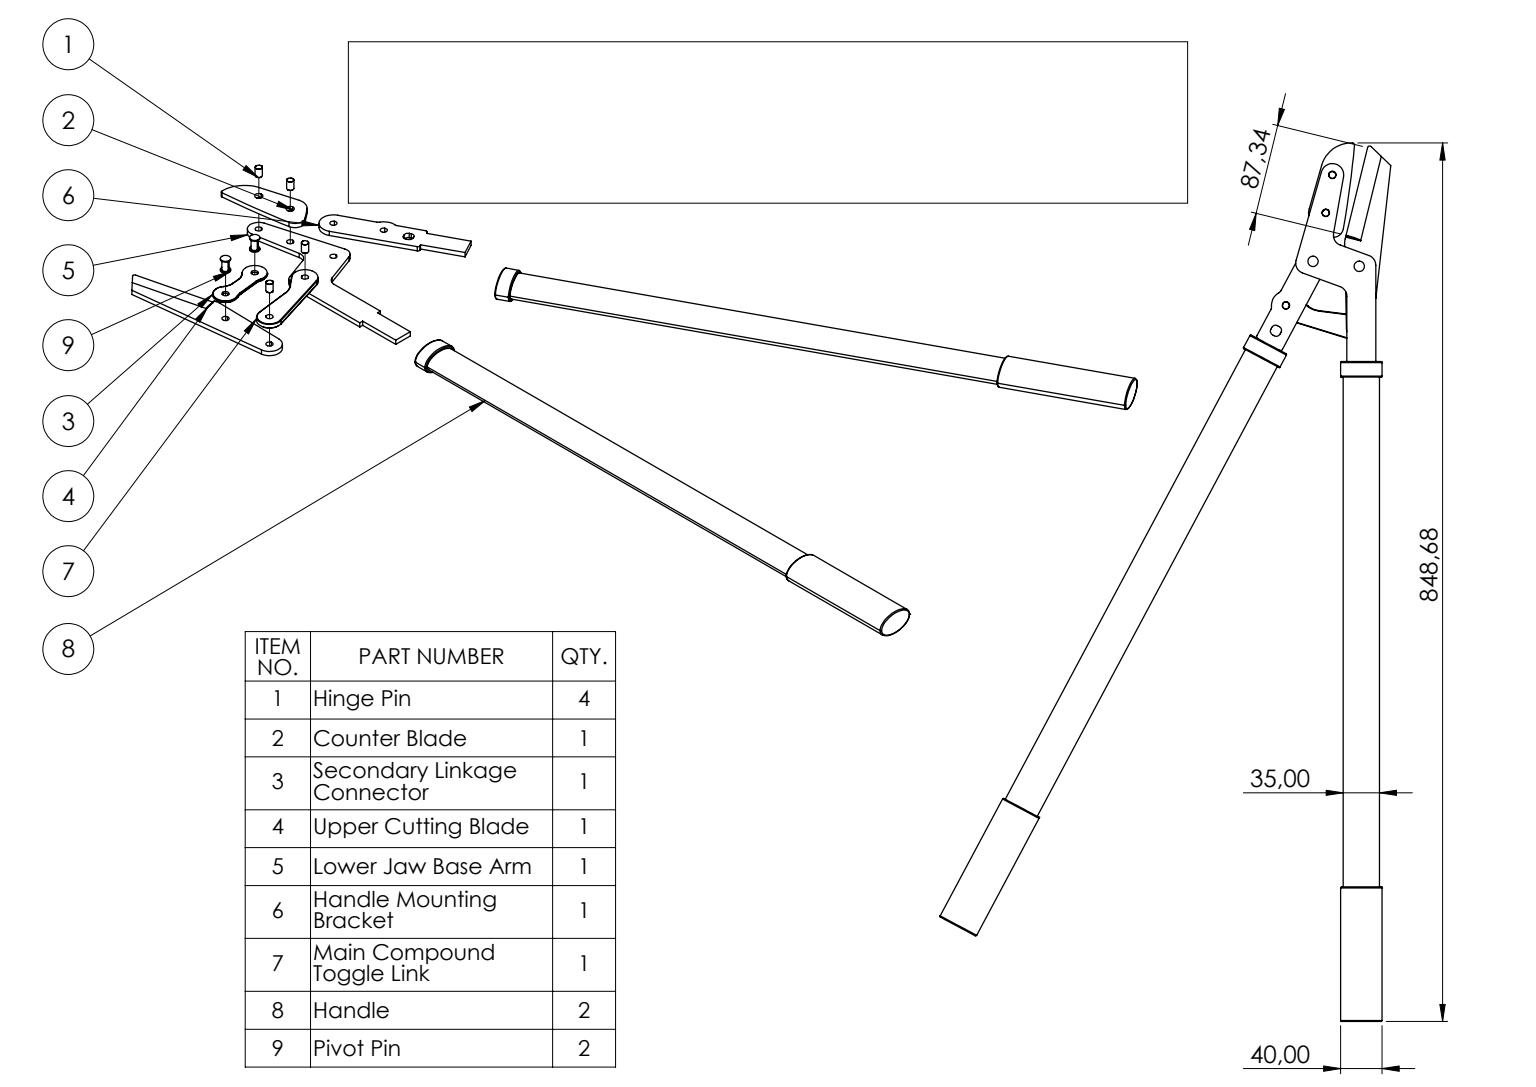
ISO-10303-21;
HEADER;
FILE_DESCRIPTION (('STEP AP214'),
    '1' );
FILE_NAME ('MAS-686',
    '2026-10-06T08:24:18',
    ( '' ),
    ( '' ),
    'SwSTEP 2.0',
    'SolidWorks 2020',
    '' );
FILE_SCHEMA (( 'AUTOMOTIVE_DESIGN' ));
ENDSEC;

DATA;
#1 = B_SPLINE_CURVE_WITH_KNOTS ( 'NONE', 3,
 ( #1947, #5214, #5583, #6285 ),
 .UNSPECIFIED., .F., .F.,
 ( 4, 4 ),
 ( 0.000000000000000000, 1.000000000000000000 ),
 .UNSPECIFIED. ) ;
#2 = DIRECTION ( 'NONE',  ( -0.000000000000000000, 1.000000000000000000, 0.000000000000000000 ) ) ;
#3 = AXIS2_PLACEMENT_3D ( 'NONE', #1835, #8382, #7525 ) ;
#4 = CARTESIAN_POINT ( 'NONE',  ( 15.24035984457677628, 4.192874667847209302, 315.0000000000000000 ) ) ;
#5 = CARTESIAN_POINT ( 'NONE',  ( 9.254661647337838914, -11.09380704494734360, -303.4999999999996589 ) ) ;
#6 = CARTESIAN_POINT ( 'NONE',  ( 16.58659719219999928, 2.947707964209000053, -314.6383426456000052 ) ) ;
#7 = SURFACE_SIDE_STYLE ('',( #8873 ) ) ;
#8 = CARTESIAN_POINT ( 'NONE',  ( -14.98500449093754483, -6.750000000000000000, -438.4247239981262396 ) ) ;
#9 = CARTESIAN_POINT ( 'NONE',  ( -1.582652182125599660, -2.660653890702000091, -435.1382991101020821 ) ) ;
#10 = ORIENTED_EDGE ( 'NONE', *, *, #9690, .T. ) ;
#11 = CARTESIAN_POINT ( 'NONE',  ( 14.97796429264999141, 8.396158284077998246, -317.0792622552969533 ) ) ;
#12 = AXIS2_PLACEMENT_3D ( 'NONE', #3802, #4074, #7998 ) ;
#13 = LINE ( 'NONE', #6569, #9092 ) ;
#14 = APPLICATION_CONTEXT ( 'automotive_design' ) ;
#15 = CARTESIAN_POINT ( 'NONE',  ( 4.345375235838000449, -11.20786428128000090, 320.0000000000000000 ) ) ;
#16 = CARTESIAN_POINT ( 'NONE',  ( -1.663986357696749074, -7.359447597713999478, -434.8428272099179708 ) ) ;
#17 = UNCERTAINTY_MEASURE_WITH_UNIT (LENGTH_MEASURE( 1.000000000000000082E-05 ), #9490, 'distance_accuracy_value', 'NONE');
#18 = CARTESIAN_POINT ( 'NONE',  ( -18.02719435607597021, -9.000000000000001776, -431.8467903975401896 ) ) ;
#19 = CARTESIAN_POINT ( 'NONE',  ( 12.11078853722071180, -6.646648371397081867, -315.0000000000000000 ) ) ;
#20 = ORIENTED_EDGE ( 'NONE', *, *, #8443, .F. ) ;
#21 = PLANE ( 'NONE',  #9517 ) ;
#22 = VERTEX_POINT ( 'NONE', #5856 ) ;
#23 = CARTESIAN_POINT ( 'NONE',  ( -16.90341843474000072, 5.241942252742000541, -317.4999999999989768 ) ) ;
#24 = VERTEX_POINT ( 'NONE', #8281 ) ;
#25 = AXIS2_PLACEMENT_3D ( 'NONE', #9737, #2431, #8928 ) ;
#26 = CARTESIAN_POINT ( 'NONE',  ( -6.686361683900003072, -11.78513185998999546, -303.6197174156509391 ) ) ;
#27 = EDGE_CURVE ( 'NONE', #6443, #1984, #9042, .T. ) ;
#28 = CARTESIAN_POINT ( 'NONE',  ( 9.022589772749004311, -9.990182113135000819, -317.4928077629770087 ) ) ;
#29 = CARTESIAN_POINT ( 'NONE',  ( 10.00000000000000000, 2.500000000000000000, -317.5000000000000000 ) ) ;
#30 = EDGE_CURVE ( 'NONE', #1105, #135, #3775, .T. ) ;
#31 = CARTESIAN_POINT ( 'NONE',  ( -18.56223039349998771, 4.700611568415998143, -303.6197174156520759 ) ) ;
#32 = CARTESIAN_POINT ( 'NONE',  ( -17.50000003227012613, 5.857864393370423528, 314.9999999999999432 ) ) ;
#33 = SHAPE_REPRESENTATION ( 'Main Compound Toggle Link', ( #2817 ), #8667 ) ;
#34 = EDGE_LOOP ( 'NONE', ( #2547, #9848, #2016, #7759 ) ) ;
#35 = DIRECTION ( 'NONE',  ( -1.000000000000000000, 0.000000000000000000, 0.000000000000000000 ) ) ;
#36 = EDGE_CURVE ( 'NONE', #6471, #8445, #5902, .T. ) ;
#37 = DIRECTION ( 'NONE',  ( 0.000000000000000000, 1.000000000000000000, 0.000000000000000000 ) ) ;
#38 = ORIENTED_EDGE ( 'NONE', *, *, #7830, .T. ) ;
#39 = AXIS2_PLACEMENT_3D ( 'NONE', #1560, #10582, #8863 ) ;
#40 = CARTESIAN_POINT ( 'NONE',  ( 16.39637408479998726, -7.274214857915000998, 190.4207385301700128 ) ) ;
#41 = DIRECTION ( 'NONE',  ( 0.000000000000000000, 0.000000000000000000, 1.000000000000000000 ) ) ;
#42 = CARTESIAN_POINT ( 'NONE',  ( 16.31080841943641602, 2.657385524587721370, -314.9999999999999432 ) ) ;
#43 = DIRECTION ( 'NONE',  ( 0.000000000000000000, -1.000000000000000000, 0.000000000000000000 ) ) ;
#44 = VECTOR ( 'NONE', #4470, 1000.000000000000114 ) ;
#45 = CARTESIAN_POINT ( 'NONE',  ( 17.36938240862999905, -0.02134527931159000205, 314.6383426456000052 ) ) ;
#46 = SHAPE_REPRESENTATION_RELATIONSHIP ( 'NONE' , 'NONE' ,  #1832, #4657 ) ;
#47 = ADVANCED_FACE ( 'NONE', ( #10008 ), #1731, .T. ) ;
#48 = CARTESIAN_POINT ( 'NONE',  ( -41.35482467236845139, -12.00000000000000000, -366.8119992166446650 ) ) ;
#49 = VECTOR ( 'NONE', #6191, 1000.000000000000000 ) ;
#50 = CARTESIAN_POINT ( 'NONE',  ( 15.30440697208000600, -7.531500302410004011, 320.0770942683900557 ) ) ;
#51 = CARTESIAN_POINT ( 'NONE',  ( -26.31853765676889267, -8.000000000000000000, -432.7407288192795249 ) ) ;
#52 = CARTESIAN_POINT ( 'NONE',  ( -19.86889125890001395, 1.746333262808030584, -303.4999999999990905 ) ) ;
#53 = CARTESIAN_POINT ( 'NONE',  ( 15.71297435277999810, 3.490404421959999670, 315.0848619657999734 ) ) ;
#54 = ORIENTED_EDGE ( 'NONE', *, *, #9742, .F. ) ;
#55 = CARTESIAN_POINT ( 'NONE',  ( 12.16184652991773163, -9.933083713569276441, 190.9999999999995737 ) ) ;
#56 = VERTEX_POINT ( 'NONE', #5109 ) ;
#57 = AXIS2_PLACEMENT_3D ( 'NONE', #266, #1824, #2572 ) ;
#58 = CARTESIAN_POINT ( 'NONE',  ( -101.0297452788102817, -7.500000000000000000, -342.4231267849074811 ) ) ;
#59 = DIRECTION ( 'NONE',  ( -0.2951854283188042882, 0.000000000000000000, 0.9554399839384178916 ) ) ;
#60 = ITEM_DEFINED_TRANSFORMATION ( 'NONE', 'NONE', #4912,  #2817 ) ;
#61 = CARTESIAN_POINT ( 'NONE',  ( 15.00000000000000000, 0.000000000000000000, -285.0000000000000000 ) ) ;
#62 = ORIENTED_EDGE ( 'NONE', *, *, #1562, .F. ) ;
#63 = DIRECTION ( 'NONE',  ( 0.7784864941891239676, 0.000000000000000000, 0.6276613564376312127 ) ) ;
#64 = LINE ( 'NONE', #8, #382 ) ;
#65 = DIRECTION ( 'NONE',  ( -0.8820010751365716661, 0.000000000000000000, -0.4712473909295749053 ) ) ;
#66 = CARTESIAN_POINT ( 'NONE',  ( -87.43749534091338660, -7.500000000000000000, -367.8627987905216514 ) ) ;
#67 = ORIENTED_EDGE ( 'NONE', *, *, #7702, .T. ) ;
#68 = CARTESIAN_POINT ( 'NONE',  ( -16.87780931964001141, 6.722286650069999148, -316.3802825947000201 ) ) ;
#69 = CIRCLE ( 'NONE', #7777, 3.500000000000020428 ) ;
#70 = CARTESIAN_POINT ( 'NONE',  ( -13.47907531561000027, -8.083075672345000129, 320.0000000000000000 ) ) ;
#71 = CARTESIAN_POINT ( 'NONE',  ( -0.1188650835482805701, -7.653137857774001240, -434.2605423690813495 ) ) ;
#72 = DIRECTION ( 'NONE',  ( 2.134661487851416834E-05, 5.799867324353239268E-11, -0.9999999997721611411 ) ) ;
#73 = CARTESIAN_POINT ( 'NONE',  ( 2.450863364448387038, -9.399909383054028567, -315.0000000000000000 ) ) ;
#74 = VECTOR ( 'NONE', #4746, 999.9999999999998863 ) ;
#75 = ORIENTED_EDGE ( 'NONE', *, *, #5258, .T. ) ;
#76 = CARTESIAN_POINT ( 'NONE',  ( 4.551150791544315233, -9.653623619670588241, -314.5171481538503144 ) ) ;
#77 = VECTOR ( 'NONE', #6835, 1000.000000000000000 ) ;
#78 = VERTEX_POINT ( 'NONE', #124 ) ;
#79 = CARTESIAN_POINT ( 'NONE',  ( 14.32993508528999982, 7.533629911342000440, -317.5000000000000000 ) ) ;
#80 = EDGE_LOOP ( 'NONE', ( #2760, #368 ) ) ;
#81 = CIRCLE ( 'NONE', #4200, 3.500000000000006217 ) ;
#82 = CARTESIAN_POINT ( 'NONE',  ( -17.70828763765000247, -5.833668797872996414, -303.6197174156520759 ) ) ;
#83 = CLOSED_SHELL ( 'NONE', ( #10215, #9940, #6869, #5277, #4807 ) ) ;
#84 = CARTESIAN_POINT ( 'NONE',  ( 3.630810623869999976, -11.17897874952999793, -317.4928077629770087 ) ) ;
#85 = DIRECTION ( 'NONE',  ( 0.000000000000000000, -1.000000000000000000, 0.000000000000000000 ) ) ;
#86 = VECTOR ( 'NONE', #9017, 1000.000000000000000 ) ;
#87 = AXIS2_PLACEMENT_3D ( 'NONE', #9230, #1862, #35 ) ;
#88 = EDGE_CURVE ( 'NONE', #8095, #9479, #7286, .T. ) ;
#89 = CARTESIAN_POINT ( 'NONE',  ( -2.737771089256917811, -7.372713325221263325, -435.0800118814183861 ) ) ;
#90 = CARTESIAN_POINT ( 'NONE',  ( -6.594989095229207621, -2.500000000000000000, -526.5005977704149700 ) ) ;
#91 = EDGE_LOOP ( 'NONE', ( #1793, #4916 ) ) ;
#92 = CARTESIAN_POINT ( 'NONE',  ( -10.00000000000000000, 2.500000000000000000, -315.0000000000000000 ) ) ;
#93 = CARTESIAN_POINT ( 'NONE',  ( 7.420201433257000545, -2.500000000000000000, -419.8948508258000061 ) ) ;
#94 = EDGE_LOOP ( 'NONE', ( #5171, #2891 ) ) ;
#95 = CARTESIAN_POINT ( 'NONE',  ( 18.68134283559999531, -4.475435185431997809, 191.1197171614399792 ) ) ;
#96 = CARTESIAN_POINT ( 'NONE',  ( -102.0103468492230547, -7.500000000000000000, -289.6591388711787545 ) ) ;
#97 = CARTESIAN_POINT ( 'NONE',  ( -1.873948611767810357, -7.500000000000000000, -349.2478646809746579 ) ) ;
#98 = DIRECTION ( 'NONE',  ( -0.9848077530122131273, 0.000000000000000000, -0.1736481776669018817 ) ) ;
#99 = CARTESIAN_POINT ( 'NONE',  ( -7.781240562249999826, 11.51887802030999985, 191.1197171614399792 ) ) ;
#100 = ORIENTED_CLOSED_SHELL ( 'NONE', *, #3850, .F. );
#101 = ADVANCED_FACE ( 'NONE', ( #5000 ), #2827, .T. ) ;
#102 =( REPRESENTATION_RELATIONSHIP ('NONE','NONE', #8468, #5180 ) REPRESENTATION_RELATIONSHIP_WITH_TRANSFORMATION ( #60 )SHAPE_REPRESENTATION_RELATIONSHIP( ) );
#103 = CARTESIAN_POINT ( 'NONE',  ( -76.74404526914973701, -12.00000000000000000, -359.2961792914830426 ) ) ;
#104 = CARTESIAN_POINT ( 'NONE',  ( -46.74071243419621169, -8.000000000000000000, -414.3237589990241077 ) ) ;
#105 = CARTESIAN_POINT ( 'NONE',  ( 18.85102544288001170, -0.8044398135754999846, 319.9928079742500131 ) ) ;
#106 = CARTESIAN_POINT ( 'NONE',  ( -9.994972990543319113, 8.217268623422803842, 314.4999428952269227 ) ) ;
#107 = CARTESIAN_POINT ( 'NONE',  ( 8.519003879469000395, 8.390442916014999142, 314.8616023057000461 ) ) ;
#108 = ORIENTED_EDGE ( 'NONE', *, *, #6819, .T. ) ;
#109 = CARTESIAN_POINT ( 'NONE',  ( 7.783073706837757122, -11.52583533951409756, 190.9999999999995737 ) ) ;
#110 = EDGE_LOOP ( 'NONE', ( #3310, #285 ) ) ;
#111 = VERTEX_POINT ( 'NONE', #3400 ) ;
#112 = AXIS2_PLACEMENT_3D ( 'NONE', #9166, #1044, #3415 ) ;
#113 = EDGE_CURVE ( 'NONE', #8766, #6326, #6244, .T. ) ;
#114 = EDGE_CURVE ( 'NONE', #1984, #5924, #1786, .T. ) ;
#115 = CARTESIAN_POINT ( 'NONE',  ( -11.58158374908019894, -4.051769059165300391, -438.8373653579053553 ) ) ;
#116 = CARTESIAN_POINT ( 'NONE',  ( -3.309867371927075919, 9.320876041153052682, 315.0000000000000568 ) ) ;
#117 = DIRECTION ( 'NONE',  ( -0.2381566831044910626, 0.000000000000000000, 0.9712267471052612455 ) ) ;
#118 = EDGE_LOOP ( 'NONE', ( #3514, #10461 ) ) ;
#119 = CARTESIAN_POINT ( 'NONE',  ( -0.6964476799210029823, -2.503143587811580861, -434.2208226102950448 ) ) ;
#120 = CARTESIAN_POINT ( 'NONE',  ( -77.67426137820133647, -2.500000000000000000, -345.8174414091573681 ) ) ;
#121 = EDGE_CURVE ( 'NONE', #3834, #7812, #4021, .T. ) ;
#122 = CARTESIAN_POINT ( 'NONE',  ( -46.74071243419621169, -8.000000000000000000, -414.3237589990241077 ) ) ;
#123 = CARTESIAN_POINT ( 'NONE',  ( 0.000000000000000000, 7.937240849781000307, 315.0000000000001705 ) ) ;
#124 = CARTESIAN_POINT ( 'NONE',  ( -5.273242226636224217, -2.500000000000000000, -350.0814130718403590 ) ) ;
#125 = CARTESIAN_POINT ( 'NONE',  ( 1.606003227921999343, 12.55439432250999587, -317.0792622552969533 ) ) ;
#126 = FACE_OUTER_BOUND ( 'NONE', #6487, .T. ) ;
#127 = CARTESIAN_POINT ( 'NONE',  ( 8.445486755484310493, -5.763031266960239485, -525.6917925150787596 ) ) ;
#128 = UNCERTAINTY_MEASURE_WITH_UNIT (LENGTH_MEASURE( 1.000000000000000082E-05 ), #4984, 'distance_accuracy_value', 'NONE');
#129 = CARTESIAN_POINT ( 'NONE',  ( -14.11853184716549059, -5.586257366442001882, -439.2418799830686567 ) ) ;
#130 = CARTESIAN_POINT ( 'NONE',  ( 16.45380452100018331, -2.370995337294541372, -315.0000000000000000 ) ) ;
#131 = ORIENTED_EDGE ( 'NONE', *, *, #4319, .T. ) ;
#132 = DIRECTION ( 'NONE',  ( -0.4712473909295827323, 0.000000000000000000, 0.8820010751365675583 ) ) ;
#133 = ORIENTED_EDGE ( 'NONE', *, *, #10090, .F. ) ;
#134 = CYLINDRICAL_SURFACE ( 'NONE', #3984, 15.00000000000001776 ) ;
#135 = VERTEX_POINT ( 'NONE', #4262 ) ;
#136 = CARTESIAN_POINT ( 'NONE',  ( 3.426853146664001759, -12.32346385046998627, -303.6197174156509391 ) ) ;
#137 = CARTESIAN_POINT ( 'NONE',  ( -10.06352840551000050, -9.619263554820991047, -317.4928077629770087 ) ) ;
#138 = EDGE_CURVE ( 'NONE', #9192, #3634, #10595, .T. ) ;
#139 = CARTESIAN_POINT ( 'NONE',  ( -16.90798586812000082, -0.2930809059028999797, -315.0848619657999734 ) ) ;
#140 = AXIS2_PLACEMENT_3D ( 'NONE', #9839, #705, #3977 ) ;
#141 = CARTESIAN_POINT ( 'NONE',  ( -5.044863629634003921, 12.10215170741999557, -303.6197174156520759 ) ) ;
#142 = CARTESIAN_POINT ( 'NONE',  ( -15.42236150774597903, -4.758481132285194981, 314.4999482133869719 ) ) ;
#143 = EDGE_LOOP ( 'NONE', ( #5687, #4056 ) ) ;
#144 = DIRECTION ( 'NONE',  ( 0.000000000000000000, -1.000000000000000000, 0.000000000000000000 ) ) ;
#145 = CARTESIAN_POINT ( 'NONE',  ( -12.36246450207000080, 8.718211867489999989, -302.5000000000000000 ) ) ;
#146 = VERTEX_POINT ( 'NONE', #9795 ) ;
#147 = CARTESIAN_POINT ( 'NONE',  ( 17.61637523988000353, -5.923742513492005202, 191.1197171614399792 ) ) ;
#148 = CARTESIAN_POINT ( 'NONE',  ( -12.98706127646999953, -6.788989183774999603, -315.0000000000001137 ) ) ;
#149 = CARTESIAN_POINT ( 'NONE',  ( 15.88699210612483803, 3.373196549223925533, -315.0000000000000000 ) ) ;
#150 = DIRECTION ( 'NONE',  ( 0.000000000000000000, 1.000000000000000000, -0.000000000000000000 ) ) ;
#151 = CARTESIAN_POINT ( 'NONE',  ( 13.05089818882000507, 9.570190452814999915, 190.4207385301700128 ) ) ;
#152 = ADVANCED_FACE ( 'NONE', ( #1627 ), #8180, .F. ) ;
#153 = CARTESIAN_POINT ( 'NONE',  ( 17.12432750374000179, 0.4000877216259000058, 314.8616023057000461 ) ) ;
#154 = LINE ( 'NONE', #4186, #6919 ) ;
#155 = CARTESIAN_POINT ( 'NONE',  ( -18.77022956583000735, -3.456581952569002247, 320.0770942683900557 ) ) ;
#156 = CARTESIAN_POINT ( 'NONE',  ( -17.50000000000000000, 1.896400240175167841E-08, 314.4999014931028682 ) ) ;
#157 = CARTESIAN_POINT ( 'NONE',  ( -19.99979308783253273, 0.5741528085765136291, -303.4999999999998863 ) ) ;
#158 = PRODUCT_RELATED_PRODUCT_CATEGORY ( 'part', '', ( #6035 ) ) ;
#159 = CARTESIAN_POINT ( 'NONE',  ( 14.38384290288000145, 5.252906928686999599, 314.8616023057000461 ) ) ;
#160 = ORIENTED_EDGE ( 'NONE', *, *, #1933, .F. ) ;
#161 = CARTESIAN_POINT ( 'NONE',  ( 10.13048420337591615, -10.78707197045944355, 190.9999999999995737 ) ) ;
#162 = ORIENTED_EDGE ( 'NONE', *, *, #3321, .F. ) ;
#163 = CARTESIAN_POINT ( 'NONE',  ( -0.6354225718825003977, 12.59144946217000260, 319.5792614743400009 ) ) ;
#164 = ORIENTED_EDGE ( 'NONE', *, *, #2368, .F. ) ;
#165 = CARTESIAN_POINT ( 'NONE',  ( -3.785374802930533633, -3.175228950698999686, -436.5426513454903557 ) ) ;
#166 = CARTESIAN_POINT ( 'NONE',  ( -12.75139817577315604, 6.274227700150676768, 315.0000000000000568 ) ) ;
#167 = CYLINDRICAL_SURFACE ( 'NONE', #9611, 3.500000000000006217 ) ;
#168 = VERTEX_POINT ( 'NONE', #2701 ) ;
#169 = VECTOR ( 'NONE', #1635, 1000.000000000000000 ) ;
#170 = CARTESIAN_POINT ( 'NONE',  ( -1.502676399155497666, -2.553500183759497055, -434.6331789313892386 ) ) ;
#171 = AXIS2_PLACEMENT_3D ( 'NONE', #4801, #2329, #8768 ) ;
#172 = EDGE_CURVE ( 'NONE', #5288, #6469, #2491, .T. ) ;
#173 = CYLINDRICAL_SURFACE ( 'NONE', #2650, 0.5000000000000004441 ) ;
#174 = CARTESIAN_POINT ( 'NONE',  ( -10.10557620461820783, -6.350202160722001388, -437.2724170503247478 ) ) ;
#175 = CARTESIAN_POINT ( 'NONE',  ( 11.05300996161902560, -7.762248705067454679, 314.4999426419801694 ) ) ;
#176 = CARTESIAN_POINT ( 'NONE',  ( -0.1242360338837507489, -2.350034431637000765, -434.3027510456794857 ) ) ;
#177 = CARTESIAN_POINT ( 'NONE',  ( -26.82908671702000802, -2.500000000000000000, -441.1544246730000509 ) ) ;
#178 = CARTESIAN_POINT ( 'NONE',  ( 14.00000000000000000, 2.500000000000000000, -410.4979246179000256 ) ) ;
#179 = AXIS2_PLACEMENT_3D ( 'NONE', #8274, #10102, #4994 ) ;
#180 = CARTESIAN_POINT ( 'NONE',  ( 8.029177897429777389, -4.293198024933910339, -525.7662775258050942 ) ) ;
#181 = EDGE_CURVE ( 'NONE', #7240, #10131, #8649, .T. ) ;
#182 = CARTESIAN_POINT ( 'NONE',  ( 8.590329508774594558, -5.782842335357056385, -525.6531578069093484 ) ) ;
#183 = CARTESIAN_POINT ( 'NONE',  ( 17.50000000000000000, 0.000000000000000000, -315.0000000000000000 ) ) ;
#184 = EDGE_CURVE ( 'NONE', #2293, #830, #6252, .T. ) ;
#185 = CARTESIAN_POINT ( 'NONE',  ( 4.714169693051698751, -9.123832451407690058, -315.0000000000000000 ) ) ;
#186 = EDGE_LOOP ( 'NONE', ( #828, #1603, #62, #6851 ) ) ;
#187 = AXIS2_PLACEMENT_3D ( 'NONE', #7775, #1275, #419 ) ;
#188 = CARTESIAN_POINT ( 'NONE',  ( 13.93637444108895096, -8.981144148067276234, -316.5000000000004547 ) ) ;
#189 = VERTEX_POINT ( 'NONE', #1946 ) ;
#190 = CARTESIAN_POINT ( 'NONE',  ( -5.180828043054999554, 11.07085478567999992, -317.5000000000000000 ) ) ;
#191 = EDGE_LOOP ( 'NONE', ( #1720, #2254, #5403, #9051 ) ) ;
#192 = CARTESIAN_POINT ( 'NONE',  ( -5.254364691879999327, -12.06635523715000424, -303.6197174156520759 ) ) ;
#193 = CARTESIAN_POINT ( 'NONE',  ( 10.19016500772999656, -9.569509725303996461, -317.4928077629770087 ) ) ;
#194 = DIRECTION ( 'NONE',  ( 0.000000000000000000, 1.000000000000000000, -0.000000000000000000 ) ) ;
#195 =( NAMED_UNIT ( * ) SI_UNIT ( $, .STERADIAN. ) SOLID_ANGLE_UNIT ( ) );
#196 = CARTESIAN_POINT ( 'NONE',  ( -3.426853146664001759, 12.32346385046998627, -303.6197174156509391 ) ) ;
#197 = ADVANCED_FACE ( 'NONE', ( #5213 ), #3671, .T. ) ;
#198 = CARTESIAN_POINT ( 'NONE',  ( -76.59645255500944927, -8.000000000000000000, -359.7738992834581495 ) ) ;
#199 = VERTEX_POINT ( 'NONE', #5447 ) ;
#200 = CARTESIAN_POINT ( 'NONE',  ( -17.12450099635000100, 0.4005340032738999856, -314.8616023057000461 ) ) ;
#201 = CARTESIAN_POINT ( 'NONE',  ( -19.00000000000000000, 0.000000000000000000, -302.5000000001010108 ) ) ;
#202 = ORIENTED_EDGE ( 'NONE', *, *, #2410, .F. ) ;
#203 = CARTESIAN_POINT ( 'NONE',  ( -20.05695074155000768, 0.5616361869863997214, 190.4207385301700128 ) ) ;
#204 = CARTESIAN_POINT ( 'NONE',  ( -2.375181255485324439, -7.500000000000000888, -406.0201668106497550 ) ) ;
#205 = CARTESIAN_POINT ( 'NONE',  ( 13.92525118639320425, 5.424153755683056133, -315.0000000000000000 ) ) ;
#206 = CARTESIAN_POINT ( 'NONE',  ( 18.77789454208001985, 4.479159834667000517, 190.4207385301700128 ) ) ;
#207 = CARTESIAN_POINT ( 'NONE',  ( 15.60185585328000002, -4.689707898928999974, 314.4150829855000211 ) ) ;
#208 =( NAMED_UNIT ( * ) SI_UNIT ( $, .STERADIAN. ) SOLID_ANGLE_UNIT ( ) );
#209 = DIRECTION ( 'NONE',  ( 0.000000000000000000, -1.000000000000000000, 0.000000000000000000 ) ) ;
#210 = CARTESIAN_POINT ( 'NONE',  ( 4.335116381453002710, -11.79481621787999757, 320.0770942683900557 ) ) ;
#211 = VECTOR ( 'NONE', #3924, 1000.000000000000000 ) ;
#212 = CARTESIAN_POINT ( 'NONE',  ( -5.453155018295565704, 9.512440914238338152, 314.4999437815906731 ) ) ;
#213 = CARTESIAN_POINT ( 'NONE',  ( -19.32402384659099326, 3.348155292981251030, -303.4999999999990905 ) ) ;
#214 = CARTESIAN_POINT ( 'NONE',  ( 12.10743226551000085, 7.094093637544000686, 314.6383426456000052 ) ) ;
#215 = VERTEX_POINT ( 'NONE', #8725 ) ;
#216 = DIRECTION ( 'NONE',  ( 0.4712473909295827323, 0.000000000000000000, -0.8820010751365675583 ) ) ;
#217 = CARTESIAN_POINT ( 'NONE',  ( 4.941041030666997180, 12.20591504665998350, 319.5792614743400009 ) ) ;
#218 = AXIS2_PLACEMENT_3D ( 'NONE', #4647, #8943, #6415 ) ;
#219 = DIRECTION ( 'NONE',  ( 0.9848077530122130163, 0.000000000000000000, 0.1736481776669023813 ) ) ;
#220 = CARTESIAN_POINT ( 'NONE',  ( -7.529172669043764365, 8.513076715957524243, 315.0000000000000000 ) ) ;
#221 = ITEM_DEFINED_TRANSFORMATION ( 'NONE', 'NONE', #3549,  #2817 ) ;
#222 = DIRECTION ( 'NONE',  ( -0.9620620651437388204, 0.000000000000000000, 0.2728306852451987674 ) ) ;
#223 = VERTEX_POINT ( 'NONE', #5395 ) ;
#224 = CARTESIAN_POINT ( 'NONE',  ( -48.08064548948741646, -8.000000000000000000, -401.8957833228595860 ) ) ;
#225 = CARTESIAN_POINT ( 'NONE',  ( -72.90663470102438737, -12.40000000000001101, -371.7168990826883714 ) ) ;
#226 = EDGE_CURVE ( 'NONE', #6555, #10444, #9360, .T. ) ;
#227 = CARTESIAN_POINT ( 'NONE',  ( -6.280550016735999996, 10.85821747223999978, 190.0000000000000000 ) ) ;
#228 = CARTESIAN_POINT ( 'NONE',  ( 17.49966312145292591, -0.4461383165315541688, 314.4999388432775049 ) ) ;
#229 = AXIS2_PLACEMENT_3D ( 'NONE', #4133, #4730, #3920 ) ;
#230 = LINE ( 'NONE', #8685, #4617 ) ;
#231 = CARTESIAN_POINT ( 'NONE',  ( 10.60393767981000757, 9.400660304482000740, 190.0071920248299477 ) ) ;
#232 = DIRECTION ( 'NONE',  ( 0.9921831154218024862, -0.000000000000000000, 0.1247904863035890766 ) ) ;
#233 = EDGE_CURVE ( 'NONE', #6469, #5288, #3524, .T. ) ;
#234 = CARTESIAN_POINT ( 'NONE',  ( 7.290921060855201752, -4.384180831252638910, -525.6208113643167508 ) ) ;
#235 = EDGE_CURVE ( 'NONE', #9158, #4552, #1974, .T. ) ;
#236 = CARTESIAN_POINT ( 'NONE',  ( 7.441233258528033190, -5.633901944276541229, -525.6643399796049607 ) ) ;
#237 = UNCERTAINTY_MEASURE_WITH_UNIT (LENGTH_MEASURE( 1.000000000000000082E-05 ), #4711, 'distance_accuracy_value', 'NONE');
#238 = DIRECTION ( 'NONE',  ( -0.2381557937579781570, -1.220925210680262645E-07, 0.9712269651834695150 ) ) ;
#239 = CARTESIAN_POINT ( 'NONE',  ( -8.616488358140818704, -8.177789738293625987, -315.0000000000000000 ) ) ;
#240 = ORIENTED_EDGE ( 'NONE', *, *, #3831, .T. ) ;
#241 = DIRECTION ( 'NONE',  ( 0.8820010751365678914, 0.000000000000000000, 0.4712473909295818442 ) ) ;
#242 = CARTESIAN_POINT ( 'NONE',  ( -13.89291764776418603, -9.007512922136868383, -316.5000000000004547 ) ) ;
#243 = ORIENTED_EDGE ( 'NONE', *, *, #9605, .T. ) ;
#244 = CARTESIAN_POINT ( 'NONE',  ( -26.82908671702000802, -2.500000000000000000, -441.1544246730000509 ) ) ;
#245 = VERTEX_POINT ( 'NONE', #4539 ) ;
#246 = CARTESIAN_POINT ( 'NONE',  ( -17.62591998684001027, 4.093640041088997705, -317.4928077629770087 ) ) ;
#247 = CARTESIAN_POINT ( 'NONE',  ( 19.46922894822000316, -1.611824300579999925, -317.5770954168139610 ) ) ;
#248 = ADVANCED_FACE ( 'NONE', ( #4441 ), #9390, .T. ) ;
#249 = CARTESIAN_POINT ( 'NONE',  ( -16.41165915566000066, 2.800979832323999830, -314.8616023057000461 ) ) ;
#250 = CARTESIAN_POINT ( 'NONE',  ( -2.040571445035855636, -7.414593747479792718, -434.8398329727854730 ) ) ;
#251 = CIRCLE ( 'NONE', #9352, 3.500000000000003997 ) ;
#252 = FACE_OUTER_BOUND ( 'NONE', #958, .T. ) ;
#253 = EDGE_LOOP ( 'NONE', ( #1986, #2444 ) ) ;
#254 = SURFACE_STYLE_USAGE ( .BOTH. , #2118 ) ;
#255 = DIRECTION ( 'NONE',  ( -0.000000000000000000, 1.000000000000000000, 0.000000000000000000 ) ) ;
#256 = AXIS2_PLACEMENT_3D ( 'NONE', #918, #8989, #8337 ) ;
#257 = ORIENTED_EDGE ( 'NONE', *, *, #493, .F. ) ;
#258 = CARTESIAN_POINT ( 'NONE',  ( -7.580171359958006505, -11.65906041016999062, 190.4207385301700128 ) ) ;
#259 = DIRECTION ( 'NONE',  ( -0.4716280258120416069, 0.000000000000000000, 0.8817975988108813779 ) ) ;
#260 = CARTESIAN_POINT ( 'NONE',  ( 16.10169247195999631, -5.923112460043001626, -302.5071922382879279 ) ) ;
#261 = CARTESIAN_POINT ( 'NONE',  ( -15.61478958302000208, 7.813810907915007320, 191.1197171614399792 ) ) ;
#262 = AXIS2_PLACEMENT_3D ( 'NONE', #8998, #1740, #3461 ) ;
#263 = CARTESIAN_POINT ( 'NONE',  ( 13.50042001888999899, -6.225262767767000049, 314.6383426456000052 ) ) ;
#264 = DIRECTION ( 'NONE',  ( -1.023612789531999991E-09, -6.047396539087999167E-11, 1.000000000000000000 ) ) ;
#265 = CARTESIAN_POINT ( 'NONE',  ( 2.578726422179000721, -12.49238522902999726, 319.5792614743400009 ) ) ;
#266 = CARTESIAN_POINT ( 'NONE',  ( -28.01838671672410896, -7.500000000000000000, -497.7560445212019999 ) ) ;
#267 = CARTESIAN_POINT ( 'NONE',  ( -16.88587703871184686, 6.724495681871323960, -303.4999999999990905 ) ) ;
#268 = CARTESIAN_POINT ( 'NONE',  ( 16.95904175860000151, 2.156867278632000229, 314.6383426456000052 ) ) ;
#269 = VERTEX_POINT ( 'NONE', #6973 ) ;
#270 = CARTESIAN_POINT ( 'NONE',  ( 13.10504385913262482, -9.452822371482909602, 190.9999999999995737 ) ) ;
#271 = CARTESIAN_POINT ( 'NONE',  ( 6.490016473005998598, 11.91548699335000272, 319.5792614743400009 ) ) ;
#272 = DIRECTION ( 'NONE',  ( 5.580921735165581358E-06, -2.007400791704409772E-12, 0.9999999999844266796 ) ) ;
#273 = CARTESIAN_POINT ( 'NONE',  ( 4.934712326437797003, 9.087261561615623151, 315.0000000000000000 ) ) ;
#274 = CARTESIAN_POINT ( 'NONE',  ( -24.05731444175778577, -2.500000000000000000, -497.1993521173619683 ) ) ;
#275 = ORIENTED_EDGE ( 'NONE', *, *, #233, .F. ) ;
#276 = CARTESIAN_POINT ( 'NONE',  ( -0.6583197226283303838, -2.500002886833834204, -434.1455329896276680 ) ) ;
#277 = CARTESIAN_POINT ( 'NONE',  ( 2.585384220735000405, 11.41066401029999966, 190.0000000000000000 ) ) ;
#278 = CARTESIAN_POINT ( 'NONE',  ( -14.02804746531204749, 5.341076607092833051, -315.0000000000000000 ) ) ;
#279 = DIRECTION ( 'NONE',  ( 0.2951854283188049544, 0.000000000000000000, -0.9554399839384174475 ) ) ;
#280 = DIRECTION ( 'NONE',  ( 0.000000000000000000, 1.000000000000000000, 0.000000000000000000 ) ) ;
#281 = PRODUCT_DEFINITION_FORMATION_WITH_SPECIFIED_SOURCE ( 'ANY', '', #6035, .NOT_KNOWN. ) ;
#282 = DIRECTION ( 'NONE',  ( 0.000000000000000000, 1.000000000000000000, 0.000000000000000000 ) ) ;
#283 = DIRECTION ( 'NONE',  ( -0.000000000000000000, 1.000000000000000000, 0.000000000000000000 ) ) ;
#284 = LINE ( 'NONE', #8342, #7202 ) ;
#285 = ORIENTED_EDGE ( 'NONE', *, *, #8827, .T. ) ;
#286 = PRODUCT_DEFINITION ( 'UNKNOWN', '', #449, #10550 ) ;
#287 = CARTESIAN_POINT ( 'NONE',  ( 28.53863984632670636, -7.500000000000000000, -506.8274460463252353 ) ) ;
#288 = CARTESIAN_POINT ( 'NONE',  ( 5.323201728285183343, -12.06184864676790447, -316.5000000000004547 ) ) ;
#289 = VERTEX_POINT ( 'NONE', #1316 ) ;
#290 = CARTESIAN_POINT ( 'NONE',  ( -59.08872748607741698, -7.500000000000000000, -420.9212224720619702 ) ) ;
#291 = ORIENTED_EDGE ( 'NONE', *, *, #4224, .T. ) ;
#292 = DIRECTION ( 'NONE',  ( -2.558226603731915840E-07, 0.9999999999999674705, 3.930810334569221757E-22 ) ) ;
#293 = CIRCLE ( 'NONE', #4573, 11.99999962017000676 ) ;
#294 = CARTESIAN_POINT ( 'NONE',  ( -19.60172830838999047, -0.3498260303709999630, -317.5770954168139610 ) ) ;
#295 = PRODUCT_DEFINITION_SHAPE ( 'NONE', 'NONE',  #6660 ) ;
#296 = CARTESIAN_POINT ( 'NONE',  ( -17.56758064089999749, 0.6313722887073000001, -314.4150829855000211 ) ) ;
#297 =( BOUNDED_CURVE ( )  B_SPLINE_CURVE ( 3, ( #701, #648, #8167, #4939 ),
 .UNSPECIFIED., .F., .F. ) 
 B_SPLINE_CURVE_WITH_KNOTS ( ( 4, 4 ),
 ( 0.000000000000000000, 0.9999999989866708017 ),
 .UNSPECIFIED. ) 
 CURVE ( )  GEOMETRIC_REPRESENTATION_ITEM ( )  RATIONAL_B_SPLINE_CURVE ( ( 1.000000000000000000, 0.8029010327867776020, 0.8003084355100938962, 0.9922222081699485496 ) ) 
 REPRESENTATION_ITEM ( '' )  );
#298 = DIRECTION ( 'NONE',  ( -0.2951854283188012906, 0.000000000000000000, 0.9554399839384188908 ) ) ;
#299 = CARTESIAN_POINT ( 'NONE',  ( 17.59656075795390606, 5.807225057570236437, 315.0000000000000000 ) ) ;
#300 = ORIENTED_EDGE ( 'NONE', *, *, #1909, .T. ) ;
#301 = CARTESIAN_POINT ( 'NONE',  ( -17.35547125580999861, -4.661453509011000307, 190.0000000000000000 ) ) ;
#302 = DIRECTION ( 'NONE',  ( -0.000000000000000000, 1.000000000000000000, 0.000000000000000000 ) ) ;
#303 = APPLICATION_CONTEXT ( 'automotive_design' ) ;
#304 = ORIENTED_EDGE ( 'NONE', *, *, #2921, .F. ) ;
#305 = DIRECTION ( 'NONE',  ( 0.000000000000000000, 1.000000000000000000, 0.000000000000000000 ) ) ;
#306 = VERTEX_POINT ( 'NONE', #406 ) ;
#307 = CARTESIAN_POINT ( 'NONE',  ( -10.00000000000000000, 2.500000000000000000, -285.0000000000000000 ) ) ;
#308 = LINE ( 'NONE', #2126, #3162 ) ;
#309 = EDGE_CURVE ( 'NONE', #4938, #6833, #7633, .T. ) ;
#310 = CARTESIAN_POINT ( 'NONE',  ( 7.580171359958006505, 11.65906041016999062, 190.4207385301700128 ) ) ;
#311 = VECTOR ( 'NONE', #7522, 1000.000000000000114 ) ;
#312 = B_SPLINE_CURVE_WITH_KNOTS ( 'NONE', 3,
 ( #4614, #3005, #5310, #9407, #7889, #6280, #1335, #5207, #2093, #7044, #1228, #5260, #3810, #10313, #5359, #7836, #485, #2950, #6223, #8534, #8486 ),
 .UNSPECIFIED., .F., .F.,
 ( 4, 1, 1, 1, 2, 2, 1, 1, 1, 1, 1, 1, 2, 2, 4 ),
 ( 0.000000000000000000, 0.2499999999999730771, 0.3749999999999595879, 0.4374999999999530931, 0.4687499999999498734, 0.4999999999999465983, 0.6249999999999374944, 0.6874999999999327205, 0.7187499999999277245, 0.7343749999999221734, 0.7421874999999192868, 0.7460937499999209521, 0.7480468749999217293, 0.7499999999999225064, 1.000000000000000000 ),
 .UNSPECIFIED. ) ;
#313 = EDGE_CURVE ( 'NONE', #8716, #4497, #7817, .T. ) ;
#314 = CARTESIAN_POINT ( 'NONE',  ( -18.87180507196998747, -0.3567823988189002815, -302.5071922382879279 ) ) ;
#315 = CARTESIAN_POINT ( 'NONE',  ( -19.98292278601002181, 0.4165571180016003350, 318.8802828394900644 ) ) ;
#316 = AXIS2_PLACEMENT_3D ( 'NONE', #10425, #6337, #7104 ) ;
#317 = CARTESIAN_POINT ( 'NONE',  ( 17.13090252310000139, 0.3058267005333999977, -314.8616023057000461 ) ) ;
#318 = ADVANCED_FACE ( 'NONE', ( #569 ), #2142, .T. ) ;
#319 = CARTESIAN_POINT ( 'NONE',  ( -14.57772014836000096, 5.380605385836000565, 314.6383426456000052 ) ) ;
#320 = VERTEX_POINT ( 'NONE', #10191 ) ;
#321 = CARTESIAN_POINT ( 'NONE',  ( 14.19899178590998190, -7.472503199908998361, 190.0071920248299477 ) ) ;
#322 = ORIENTED_EDGE ( 'NONE', *, *, #2909, .F. ) ;
#323 = CARTESIAN_POINT ( 'NONE',  ( 1.330908921489000418, 12.56946842516999041, 319.5792614743400009 ) ) ;
#324 = CARTESIAN_POINT ( 'NONE',  ( -99.26574312853713877, -7.500000000000000000, -341.4806320030483562 ) ) ;
#325 = CARTESIAN_POINT ( 'NONE',  ( 9.142607798242581296, 7.997258514545670494, 315.0000000000000000 ) ) ;
#326 = LINE ( 'NONE', #4560, #9098 ) ;
#327 = DIRECTION ( 'NONE',  ( 0.000000000000000000, -1.000000000000000000, 0.000000000000000000 ) ) ;
#328 = FILL_AREA_STYLE_COLOUR ( '', #2300 ) ;
#329 = ADVANCED_FACE ( 'NONE', ( #9439 ), #3687, .F. ) ;
#330 = CARTESIAN_POINT ( 'NONE',  ( 13.37693598625000213, 8.145668871592000926, 190.0000000000000000 ) ) ;
#331 = CARTESIAN_POINT ( 'NONE',  ( 13.64750606492133045, -6.290789845814279246, 314.4999418822395114 ) ) ;
#332 = CARTESIAN_POINT ( 'NONE',  ( -15.60334176867001688, 6.376785739494004623, 190.0071920248299477 ) ) ;
#333 = DIRECTION ( 'NONE',  ( 0.000000000000000000, -1.000000000000000000, 0.000000000000000000 ) ) ;
#334 = FACE_OUTER_BOUND ( 'NONE', #8944, .T. ) ;
#335 = CIRCLE ( 'NONE', #1709, 15.00000000000001776 ) ;
#336 = CARTESIAN_POINT ( 'NONE',  ( 7.538136778550191153, -5.645663747140947208, -525.6900796742911552 ) ) ;
#337 = CARTESIAN_POINT ( 'NONE',  ( 14.25090727152774228, -5.161646102170217354, 315.0000000000000568 ) ) ;
#338 = LINE ( 'NONE', #980, #680 ) ;
#339 = ORIENTED_EDGE ( 'NONE', *, *, #9047, .F. ) ;
#340 = CARTESIAN_POINT ( 'NONE',  ( 3.092734256763002065, 11.24153629139000188, 319.9928079742500131 ) ) ;
#341 = CARTESIAN_POINT ( 'NONE',  ( -16.85039254115126539, -6.759165854037040511, -316.5000000000004547 ) ) ;
#342 = EDGE_CURVE ( 'NONE', #5251, #8235, #3736, .T. ) ;
#343 = CARTESIAN_POINT ( 'NONE',  ( -43.33032886859687949, -9.000000000000001776, -402.2979831847329706 ) ) ;
#344 = VERTEX_POINT ( 'NONE', #2396 ) ;
#345 = CARTESIAN_POINT ( 'NONE',  ( -1.873948611771682149, -8.000000000000000000, -349.2478646809681777 ) ) ;
#346 = AXIS2_PLACEMENT_3D ( 'NONE', #860, #2744, #910 ) ;
#347 = CARTESIAN_POINT ( 'NONE',  ( -14.69255688194000520, -7.987735679832996816, -317.5770954168139610 ) ) ;
#348 = CARTESIAN_POINT ( 'NONE',  ( -15.92197846796999983, 3.582977715798000062, -314.8616023057000461 ) ) ;
#349 = CARTESIAN_POINT ( 'NONE',  ( 17.27223423031419358, 1.573973318776797026, -314.5135302205612220 ) ) ;
#350 = ORIENTED_EDGE ( 'NONE', *, *, #8269, .F. ) ;
#351 = PRESENTATION_STYLE_ASSIGNMENT (( #254 ) ) ;
#352 = DIRECTION ( 'NONE',  ( 0.000000000000000000, -1.000000000000000000, 0.000000000000000000 ) ) ;
#353 = ADVANCED_FACE ( 'NONE', ( #5555 ), #5229, .T. ) ;
#354 = ORIENTED_EDGE ( 'NONE', *, *, #10397, .T. ) ;
#355 = DIRECTION ( 'NONE',  ( -0.000000000000000000, 1.000000000000000000, 0.000000000000000000 ) ) ;
#356 = EDGE_LOOP ( 'NONE', ( #3781, #10603 ) ) ;
#357 = PLANE ( 'NONE',  #5547 ) ;
#358 = CYLINDRICAL_SURFACE ( 'NONE', #9948, 4.000000000000000000 ) ;
#359 = DIRECTION ( 'NONE',  ( 0.000000000000000000, 1.000000000000000000, 0.000000000000000000 ) ) ;
#360 = CIRCLE ( 'NONE', #7394, 3.500000000000000000 ) ;
#361 = ADVANCED_FACE ( 'NONE', ( #10562 ), #4708, .F. ) ;
#362 = CARTESIAN_POINT ( 'NONE',  ( -0.5452757643750816285, -7.478314948056999256, -434.2680375005485871 ) ) ;
#363 = EDGE_CURVE ( 'NONE', #1218, #8202, #3035, .T. ) ;
#364 = FACE_OUTER_BOUND ( 'NONE', #2969, .T. ) ;
#365 = CARTESIAN_POINT ( 'NONE',  ( 19.56939737065003015, -2.860667089442002986, 319.5792614743400009 ) ) ;
#366 = DIRECTION ( 'NONE',  ( 0.000000000000000000, -1.000000000000000000, 0.000000000000000000 ) ) ;
#367 = CARTESIAN_POINT ( 'NONE',  ( -14.43094748301999886, 5.211771040651000497, 314.8616023057000461 ) ) ;
#368 = ORIENTED_EDGE ( 'NONE', *, *, #5471, .T. ) ;
#369 = DIRECTION ( 'NONE',  ( -0.000000000000000000, 1.000000000000000000, 0.000000000000000000 ) ) ;
#370 = ORIENTED_EDGE ( 'NONE', *, *, #7787, .T. ) ;
#371 = CARTESIAN_POINT ( 'NONE',  ( -17.61140045117998554, 5.929979699424000827, 318.8802828394900644 ) ) ;
#372 = CIRCLE ( 'NONE', #1744, 14.99999999999999467 ) ;
#373 = EDGE_CURVE ( 'NONE', #5743, #3634, #3350, .T. ) ;
#374 = CARTESIAN_POINT ( 'NONE',  ( -17.13182678275000370, 0.2945984483948000388, 314.8616023057000461 ) ) ;
#375 = CARTESIAN_POINT ( 'NONE',  ( -15.88661950543927404, 3.373766516133892335, 315.0000000000000000 ) ) ;
#376 = CARTESIAN_POINT ( 'NONE',  ( -63.11273421720001409, 2.500000000000000000, -415.2750182148000135 ) ) ;
#377 = CYLINDRICAL_SURFACE ( 'NONE', #3349, 3.500000000000003109 ) ;
#378 = PLANE ( 'NONE',  #9312 ) ;
#379 =( BOUNDED_SURFACE ( )  B_SPLINE_SURFACE ( 3, 3, ( 
 ( #3396, #9259, #9950, #5161, #8434, #1074, #1023, #5853, #7635, #8489 ),
 ( #9144, #5053, #8334, #972, #4258, #7528, #174, #3449, #9205, #5106 ),
 ( #4309, #3504, #2902, #7046, #4459, #8641, #8536, #5261, #1178, #6121 ),
 ( #7891, #3812, #10155, #4565, #6282, #5361, #3653, #2151, #3007, #7099 ) ),
 .UNSPECIFIED., .F., .F., .T. ) 
 B_SPLINE_SURFACE_WITH_KNOTS ( ( 4, 4 ),
 ( 4, 1, 1, 1, 1, 1, 1, 4 ),
 ( 0.000000000000000000, 1.000000000000000000 ),
 ( 0.04004302100395999708, 0.1036559982346000053, 0.2203786577267000113, 0.3496747522196999580, 0.4912411616719999929, 0.6462853912813000257, 0.8150922079746999449, 0.8736421606905999671 ),
 .UNSPECIFIED. ) 
 GEOMETRIC_REPRESENTATION_ITEM ( )  RATIONAL_B_SPLINE_SURFACE ( (
 ( 1.237064798922000053, 1.237064798922000053, 1.237064798922000053, 1.237064798922000053, 1.237064798922000053, 1.237064798922000053, 1.237064798922000053, 1.237064798922000053, 1.237064798922000053, 1.237064798922000053),
 ( 0.9209784003594999602, 0.9209784003594999602, 0.9209784003594999602, 0.9209784003594999602, 0.9209784003594999602, 0.9209784003594999602, 0.9209784003594999602, 0.9209784003594999602, 0.9209784003594999602, 0.9209784003594999602),
 ( 0.9209784003594999602, 0.9209784003594999602, 0.9209784003594999602, 0.9209784003594999602, 0.9209784003594999602, 0.9209784003594999602, 0.9209784003594999602, 0.9209784003594999602, 0.9209784003594999602, 0.9209784003594999602),
 ( 1.237064798922000053, 1.237064798922000053, 1.237064798922000053, 1.237064798922000053, 1.237064798922000053, 1.237064798922000053, 1.237064798922000053, 1.237064798922000053, 1.237064798922000053, 1.237064798922000053) ) ) 
 REPRESENTATION_ITEM ( '' )  SURFACE ( )  );
#380 = DIRECTION ( 'NONE',  ( -0.9612616959383296633, 0.000000000000000000, -0.2756373558169616933 ) ) ;
#381 = PRODUCT ( 'Main Compound Toggle Link', 'Main Compound Toggle Link', '', ( #10374 ) ) ;
#383 = CARTESIAN_POINT ( 'NONE',  ( -8.676965067697993916, 10.10010313590999509, 190.0071920248299477 ) ) ;
#382 = VECTOR ( 'NONE', #1674, 1000.000000000000114 ) ;
#384 = LINE ( 'NONE', #2047, #7288 ) ;
#385 = CARTESIAN_POINT ( 'NONE',  ( 6.150179767644408990, -4.500000000000001776, -524.6161169473078871 ) ) ;
#386 = DIRECTION ( 'NONE',  ( 0.9627070496199738869, -0.1321637200910051047, 0.2360675490272045596 ) ) ;
#387 = CARTESIAN_POINT ( 'NONE',  ( 8.517242506840645433, -8.210459489885888473, 315.0000000000000568 ) ) ;
#388 = CARTESIAN_POINT ( 'NONE',  ( 11.99990625867999938, 6.898016740823000426, -314.8616023057000461 ) ) ;
#389 = AXIS2_PLACEMENT_3D ( 'NONE', #10091, #3429, #953 ) ;
#390 = ORIENTED_EDGE ( 'NONE', *, *, #6600, .F. ) ;
#391 = CARTESIAN_POINT ( 'NONE',  ( 10.79243608611000305, 9.321647281761997306, 319.9928079742500131 ) ) ;
#392 = CARTESIAN_POINT ( 'NONE',  ( -79.04021210711869116, -7.500000000000000000, -328.4066924704651456 ) ) ;
#393 = CARTESIAN_POINT ( 'NONE',  ( -77.77979771402830522, -2.500000000000000000, -385.9384419754180158 ) ) ;
#394 = ORIENTED_EDGE ( 'NONE', *, *, #6640, .T. ) ;
#395 = CARTESIAN_POINT ( 'NONE',  ( -15.97383562432999149, -7.643564190274003245, -317.0792622552969533 ) ) ;
#396 = DIRECTION ( 'NONE',  ( -0.1071946444232961260, 0.000000000000000000, 0.9942380540931650135 ) ) ;
#397 = DIRECTION ( 'NONE',  ( -0.9554399839384177806, 0.000000000000000000, -0.2951854283188049544 ) ) ;
#398 = ORIENTED_EDGE ( 'NONE', *, *, #3468, .T. ) ;
#399 = CARTESIAN_POINT ( 'NONE',  ( 12.62255196312000116, -8.576358104672999971, 190.0000000000000000 ) ) ;
#400 = DIRECTION ( 'NONE',  ( -0.9712267471052594692, 0.000000000000000000, -0.2381566831044984178 ) ) ;
#401 = ORIENTED_EDGE ( 'NONE', *, *, #4319, .F. ) ;
#402 = CARTESIAN_POINT ( 'NONE',  ( -15.59929043073998578, -7.826471063572999931, 191.1197171614399792 ) ) ;
#403 = ORIENTED_EDGE ( 'NONE', *, *, #6734, .T. ) ;
#404 = DIRECTION ( 'NONE',  ( 0.000000000000000000, -1.000000000000000000, 0.000000000000000000 ) ) ;
#405 = CARTESIAN_POINT ( 'NONE',  ( -1.914578617915998704, -11.33709939001001032, -302.5071922382879279 ) ) ;
#406 = CARTESIAN_POINT ( 'NONE',  ( -79.74686404004059170, -2.500000000000000000, -383.9321052860355508 ) ) ;
#407 = EDGE_CURVE ( 'NONE', #146, #5498, #4519, .T. ) ;
#408 = AXIS2_PLACEMENT_3D ( 'NONE', #7213, #5750, #10480 ) ;
#409 = CARTESIAN_POINT ( 'NONE',  ( -0.7256479603086914976, -7.501867437109999592, -434.1451055704292799 ) ) ;
#410 = FILL_AREA_STYLE_COLOUR ( '', #1992 ) ;
#411 = CARTESIAN_POINT ( 'NONE',  ( -13.35956122709998795, 8.020600178289003068, -302.5071922382879279 ) ) ;
#412 = CARTESIAN_POINT ( 'NONE',  ( -19.58476356052999279, -2.818858455686998887, 319.5792614743400009 ) ) ;
#413 = CARTESIAN_POINT ( 'NONE',  ( 16.99702983282000091, -1.298346578676000007, -314.8616023057000461 ) ) ;
#414 = AXIS2_PLACEMENT_3D ( 'NONE', #9424, #292, #2763 ) ;
#415 = CARTESIAN_POINT ( 'NONE',  ( -12.17979804859000126, 7.053762231097000068, 314.6383426456000052 ) ) ;
#416 = ORIENTED_EDGE ( 'NONE', *, *, #9414, .F. ) ;
#417 = CARTESIAN_POINT ( 'NONE',  ( -9.595833218033995138, -9.789665514059997520, 190.0071920248299477 ) ) ;
#418 = CARTESIAN_POINT ( 'NONE',  ( -0.6596894340221253206, -7.499999891561000886, -434.1397621899948263 ) ) ;
#419 = DIRECTION ( 'NONE',  ( -0.9612616959383174509, 0.000000000000000000, -0.2756373558170044369 ) ) ;
#420 = AXIS2_PLACEMENT_3D ( 'NONE', #3970, #5684, #9832 ) ;
#421 = STYLED_ITEM ( 'NONE', ( #698 ), #5138 ) ;
#422 = EDGE_CURVE ( 'NONE', #306, #9067, #9592, .T. ) ;
#423 = CARTESIAN_POINT ( 'NONE',  ( -17.35477687787999912, 0.3068793820639000303, 314.6383426456000052 ) ) ;
#424 = CARTESIAN_POINT ( 'NONE',  ( -16.34899991413091414, 2.583752171356570759, 315.0000000000000000 ) ) ;
#425 = CARTESIAN_POINT ( 'NONE',  ( -84.02975002432511076, -2.500000000000000000, -342.4104245220563030 ) ) ;
#426 = AXIS2_PLACEMENT_3D ( 'NONE', #4824, #7296, #1375 ) ;
#427 = AXIS2_PLACEMENT_3D ( 'NONE', #92, #1648, #838 ) ;
#428 = CARTESIAN_POINT ( 'NONE',  ( -16.31080841943642312, -2.657385524587722703, -315.0000000000001137 ) ) ;
#429 = CARTESIAN_POINT ( 'NONE',  ( -1.582652182125599660, -2.660653890702000091, -435.1382991101020821 ) ) ;
#430 =( NAMED_UNIT ( * ) PLANE_ANGLE_UNIT ( ) SI_UNIT ( $, .RADIAN. ) );
#431 = CARTESIAN_POINT ( 'NONE',  ( 11.71572875054933327, 12.50000000135959688, -303.5000000000000000 ) ) ;
#432 = EDGE_CURVE ( 'NONE', #700, #6716, #7233, .T. ) ;
#433 = CARTESIAN_POINT ( 'NONE',  ( 8.586696445213114259, 8.187646113561793726, -314.9999999999999432 ) ) ;
#434 = CARTESIAN_POINT ( 'NONE',  ( 17.75414941409001557, 3.856242593410000197, 190.0071920248299477 ) ) ;
#435 = B_SPLINE_CURVE_WITH_KNOTS ( 'NONE', 3,
 ( #4769, #8901, #8094, #8733, #8788, #10403, #10619, #2354, #4014, #790, #6372, #2295 ),
 .UNSPECIFIED., .F., .F.,
 ( 4, 2, 2, 2, 2, 4 ),
 ( 0.000000000000000000, 0.4999999999999995559, 0.7499999999999974465, 0.8749999999999965583, 0.9374999999999983347, 1.000000000000000000 ),
 .UNSPECIFIED. ) ;
#436 = CARTESIAN_POINT ( 'NONE',  ( 17.50000000000000711, -8.653864165198663120E-10, -302.4999999999999432 ) ) ;
#437 = EDGE_CURVE ( 'NONE', #3828, #7650, #10190, .T. ) ;
#438 = ORIENTED_EDGE ( 'NONE', *, *, #6849, .T. ) ;
#439 = CARTESIAN_POINT ( 'NONE',  ( -11.26076953950000004, -9.251451169536998975, -317.5000000000000000 ) ) ;
#440 = DIRECTION ( 'NONE',  ( 1.000000000000000000, 0.000000000000000000, 0.000000000000000000 ) ) ;
#441 = DIRECTION ( 'NONE',  ( 1.000000000000000000, 0.000000000000000000, 0.000000000000000000 ) ) ;
#442 = CARTESIAN_POINT ( 'NONE',  ( 2.737672117484407863, -9.377292971636139285, 315.0000000000000568 ) ) ;
#443 = CARTESIAN_POINT ( 'NONE',  ( 13.18712987686000027, 5.898505050745000311, -315.0848619657999734 ) ) ;
#444 = EDGE_CURVE ( 'NONE', #7016, #4872, #3088, .T. ) ;
#445 = CARTESIAN_POINT ( 'NONE',  ( 18.45919443845001950, 2.405475664342000996, 319.9928079742500131 ) ) ;
#446 = CARTESIAN_POINT ( 'NONE',  ( -0.6528312677253685914, -7.479800707286198502, -434.5251259939439024 ) ) ;
#447 = CARTESIAN_POINT ( 'NONE',  ( -5.500000000000000000, 2.500000000000000000, -409.5000000000000568 ) ) ;
#448 = ORIENTED_EDGE ( 'NONE', *, *, #9438, .T. ) ;
#449 = PRODUCT_DEFINITION_FORMATION_WITH_SPECIFIED_SOURCE ( 'ANY', '', #8602, .NOT_KNOWN. ) ;
#450 = CARTESIAN_POINT ( 'NONE',  ( 19.39427072114999717, -3.381181012882998882, -317.0792622552969533 ) ) ;
#451 = CARTESIAN_POINT ( 'NONE',  ( -14.96977070983867009, -9.000000000000001776, -385.2505660326773409 ) ) ;
#452 = B_SPLINE_CURVE_WITH_KNOTS ( 'NONE', 3,
 ( #9871, #3367, #5940, #9919, #5772, #2557, #9228, #142, #5825, #942, #10323, #1912, #8408, #5184, #1349, #10377, #4385, #5129, #7659, #8654, #4578, #3528 ),
 .UNSPECIFIED., .F., .F.,
 ( 4, 2, 2, 2, 2, 2, 2, 2, 2, 2, 4 ),
 ( 0.000000000000000000, 0.06249979490446620767, 0.1249995898089324153, 0.1874993847133986091, 0.2499991796178648307, 0.3124989745223310522, 0.3437488719745641630, 0.3749987694267972183, 0.4062486668790303290, 0.4374985643312634398, 0.4999983592357296613 ),
 .UNSPECIFIED. ) ;
#453 = ADVANCED_BREP_SHAPE_REPRESENTATION ( '', ( #5170, #2817 ), #8168 ) ;
#454 = CARTESIAN_POINT ( 'NONE',  ( 9.378959784071181360, -5.899999999999999467, -525.1866552614185366 ) ) ;
#455 = ORIENTED_EDGE ( 'NONE', *, *, #1550, .F. ) ;
#456 = CARTESIAN_POINT ( 'NONE',  ( -14.18540515794000001, -7.627402598852000004, 190.0000000000000000 ) ) ;
#457 = EDGE_CURVE ( 'NONE', #8095, #5909, #7178, .T. ) ;
#458 = ORIENTED_EDGE ( 'NONE', *, *, #4238, .T. ) ;
#459 = CARTESIAN_POINT ( 'NONE',  ( 10.12800840543000724, -10.78031690431999756, 191.1197171614399792 ) ) ;
#460 = ORIENTED_EDGE ( 'NONE', *, *, #1348, .F. ) ;
#461 = CARTESIAN_POINT ( 'NONE',  ( -16.68818136459866253, -1.819152193222137281, 315.0000000000000000 ) ) ;
#462 = CARTESIAN_POINT ( 'NONE',  ( 13.35956122709998795, -8.020600178289003068, -302.5071922382879279 ) ) ;
#463 = DIRECTION ( 'NONE',  ( 0.000000000000000000, 1.000000000000000000, 0.000000000000000000 ) ) ;
#464 = CARTESIAN_POINT ( 'NONE',  ( -1.658294475769471310, -7.463038962712998270, -434.6370517716558197 ) ) ;
#465 =( LENGTH_UNIT ( ) NAMED_UNIT ( * ) SI_UNIT ( .MILLI., .METRE. ) );
#466 = CARTESIAN_POINT ( 'NONE',  ( 6.445894847559003438, 10.69844988487999693, -302.5071922382879279 ) ) ;
#467 = PRODUCT_DEFINITION_SHAPE ( 'NONE', 'NONE',  #286 ) ;
#468 = CARTESIAN_POINT ( 'NONE',  ( -16.43550475785002263, -7.239471399781003846, 319.5792614743400009 ) ) ;
#469 = CARTESIAN_POINT ( 'NONE',  ( 15.92197846796999983, -3.582977715798000062, -314.8616023057000461 ) ) ;
#470 = CARTESIAN_POINT ( 'NONE',  ( -13.62823431091000081, 6.408810695481999886, 314.4150829855000211 ) ) ;
#471 = VERTEX_POINT ( 'NONE', #3146 ) ;
#472 = CARTESIAN_POINT ( 'NONE',  ( 17.73236801841998300, -3.892024484092002634, 190.0071920248299477 ) ) ;
#473 = ORIENTED_EDGE ( 'NONE', *, *, #1711, .T. ) ;
#474 = CIRCLE ( 'NONE', #7341, 4.000000000000008882 ) ;
#475 = CARTESIAN_POINT ( 'NONE',  ( -1.788249073448326953, -7.429140679109920598, -434.7441729133906279 ) ) ;
#476 = CARTESIAN_POINT ( 'NONE',  ( -78.61675616006050404, -7.500000000000000000, -344.0534392588842252 ) ) ;
#477 = ADVANCED_FACE ( 'NONE', ( #9646 ), #582, .T. ) ;
#478 = FACE_OUTER_BOUND ( 'NONE', #9284, .T. ) ;
#479 = CARTESIAN_POINT ( 'NONE',  ( -30.41084982323499730, -2.500000000000000000, -460.5301199443746327 ) ) ;
#480 = CIRCLE ( 'NONE', #7844, 3.500000000000003109 ) ;
#481 = PRODUCT_RELATED_PRODUCT_CATEGORY ( 'part', '', ( #8602 ) ) ;
#482 = CARTESIAN_POINT ( 'NONE',  ( -16.61594764501906596, 2.013242305049250280, 315.0000000000001137 ) ) ;
#483 = DIRECTION ( 'NONE',  ( -0.000000000000000000, 1.000000000000000000, 0.000000000000000000 ) ) ;
#484 = CARTESIAN_POINT ( 'NONE',  ( -10.90988923471838667, -7.272053090123304031, -315.0000000000000568 ) ) ;
#485 = CARTESIAN_POINT ( 'NONE',  ( -3.771252382897392952, -2.975477256776445145, -436.1454489244006822 ) ) ;
#486 = CARTESIAN_POINT ( 'NONE',  ( -79.74686404004059170, -7.500000000000000000, -383.9321052860355508 ) ) ;
#487 = CARTESIAN_POINT ( 'NONE',  ( 17.50000000088855501, 5.867334121986936601, -302.4999999999996589 ) ) ;
#488 = CARTESIAN_POINT ( 'NONE',  ( 0.9838506439437809670, 9.488399989288442526, -314.9999999999998863 ) ) ;
#489 = CARTESIAN_POINT ( 'NONE',  ( -19.54676335584001023, 0.8901129224502002391, 189.9229057364800042 ) ) ;
#490 = CARTESIAN_POINT ( 'NONE',  ( 11.54127216423516877, 7.525448809341461320, 314.4999468205385824 ) ) ;
#491 = ORIENTED_EDGE ( 'NONE', *, *, #8849, .T. ) ;
#492 = CARTESIAN_POINT ( 'NONE',  ( -36.01445213885307339, -7.500000000000000000, -460.8005622778243264 ) ) ;
#493 = EDGE_CURVE ( 'NONE', #7563, #4961, #4707, .T. ) ;
#494 = LINE ( 'NONE', #3762, #7350 ) ;
#495 = DIRECTION ( 'NONE',  ( 0.000000000000000000, 0.000000000000000000, 1.000000000000000000 ) ) ;
#496 = CARTESIAN_POINT ( 'NONE',  ( 9.217211940708146756, -7.977736869146946574, 315.0000000000000000 ) ) ;
#497 = CARTESIAN_POINT ( 'NONE',  ( -8.551447359560999217, 8.144527334518999240, -315.0848619657999734 ) ) ;
#498 = PLANE ( 'NONE',  #1895 ) ;
#499 = CARTESIAN_POINT ( 'NONE',  ( -18.12318599310000167, 3.186119256560000945, 319.9928079742500131 ) ) ;
#500 = CARTESIAN_POINT ( 'NONE',  ( -2.000000000000000000, 2.500000000000000000, -414.5000000000000000 ) ) ;
#501 = CARTESIAN_POINT ( 'NONE',  ( -0.5293798494821438938, -2.512522400030999137, -434.0497706731864582 ) ) ;
#502 = EDGE_LOOP ( 'NONE', ( #7761, #10328 ) ) ;
#503 = CARTESIAN_POINT ( 'NONE',  ( -18.21319838702001448, 4.476589323548002319, -317.5770954168139610 ) ) ;
#504 = CARTESIAN_POINT ( 'NONE',  ( -11.69962851017000283, -10.23591410519999201, -317.0792622552969533 ) ) ;
#505 = ADVANCED_FACE ( 'NONE', ( #3252 ), #1591, .F. ) ;
#506 = DIRECTION ( 'NONE',  ( 1.000000000000000000, 0.000000000000000000, 0.000000000000000000 ) ) ;
#507 = EDGE_CURVE ( 'NONE', #6146, #7283, #8033, .T. ) ;
#508 = CARTESIAN_POINT ( 'NONE',  ( -17.50000000000000000, 0.000000000000000000, -315.0000000000000000 ) ) ;
#509 = EDGE_LOOP ( 'NONE', ( #4732, #10118, #10336, #1157 ) ) ;
#510 = CARTESIAN_POINT ( 'NONE',  ( -12.62255196312000116, 8.576358104672999971, 190.0000000000000000 ) ) ;
#511 = VECTOR ( 'NONE', #4805, 1000.000000000000000 ) ;
#512 = AXIS2_PLACEMENT_3D ( 'NONE', #1643, #10610, #2448 ) ;
#513 = DIRECTION ( 'NONE',  ( 0.000000000000000000, 0.000000000000000000, 1.000000000000000000 ) ) ;
#514 = VERTEX_POINT ( 'NONE', #8144 ) ;
#515 = CARTESIAN_POINT ( 'NONE',  ( -19.78498824058000594, -1.878712957033002340, 191.1197171614399792 ) ) ;
#516 = ORIENTED_EDGE ( 'NONE', *, *, #3831, .F. ) ;
#517 = FACE_OUTER_BOUND ( 'NONE', #2695, .T. ) ;
#518 = CARTESIAN_POINT ( 'NONE',  ( 10.36918760129999484, -10.25095399663999451, -302.4229045757450081 ) ) ;
#519 = DIRECTION ( 'NONE',  ( -0.000000000000000000, 1.000000000000000000, 0.000000000000000000 ) ) ;
#520 = AXIS2_PLACEMENT_3D ( 'NONE', #3309, #8355, #7553 ) ;
#521 = CARTESIAN_POINT ( 'NONE',  ( -0.9182485701526132971, -7.496877080320997422, -434.3056557713407528 ) ) ;
#522 = FILL_AREA_STYLE_COLOUR ( '', #3538 ) ;
#523 = CARTESIAN_POINT ( 'NONE',  ( -6.297776810737998332, 10.73166643879000404, -302.5071922382879279 ) ) ;
#524 = DIRECTION ( 'NONE',  ( 0.000000000000000000, 0.000000000000000000, -1.000000000000000000 ) ) ;
#525 = CARTESIAN_POINT ( 'NONE',  ( -17.14577796628000073, 0.02050488658304999712, 314.8616023057000461 ) ) ;
#526 = ORIENTED_EDGE ( 'NONE', *, *, #7256, .F. ) ;
#527 = DIRECTION ( 'NONE',  ( 0.2951854283188045658, 0.000000000000000000, -0.9554399839384175586 ) ) ;
#528 = CARTESIAN_POINT ( 'NONE',  ( -16.98888588455999127, 6.600739700975996271, 318.8802828394900644 ) ) ;
#529 = CIRCLE ( 'NONE', #6531, 14.00000000000000888 ) ;
#530 = DIRECTION ( 'NONE',  ( 0.000000000000000000, 0.000000000000000000, 1.000000000000000000 ) ) ;
#531 = STYLED_ITEM ( 'NONE', ( #3235 ), #1856 ) ;
#532 = LINE ( 'NONE', #2793, #8706 ) ;
#533 = DIRECTION ( 'NONE',  ( 0.000000000000000000, -1.000000000000000000, 0.000000000000000000 ) ) ;
#534 = CARTESIAN_POINT ( 'NONE',  ( 11.28781796570999951, -4.951468039558000633, 315.0000000000001705 ) ) ;
#535 = CARTESIAN_POINT ( 'NONE',  ( -13.94567317170587017, -5.407789506212602682, -314.9999999999999432 ) ) ;
#536 = CARTESIAN_POINT ( 'NONE',  ( -86.49427212956700828, -7.500000000000000000, -350.5299153184531633 ) ) ;
#537 = LINE ( 'NONE', #9560, #754 ) ;
#538 = CARTESIAN_POINT ( 'NONE',  ( -10.23467949692583190, 10.00000000050611959, -302.5000000000002842 ) ) ;
#539 = CARTESIAN_POINT ( 'NONE',  ( 8.377487131979357571, 8.255758461348163380, -315.0000000000000000 ) ) ;
#540 = CARTESIAN_POINT ( 'NONE',  ( -20.05687582562997662, -0.5621360437329007143, 190.4207385301700128 ) ) ;
#541 = CARTESIAN_POINT ( 'NONE',  ( -76.59645255681878950, -12.50000000000000000, -359.7738992776017994 ) ) ;
#542 = CARTESIAN_POINT ( 'NONE',  ( 9.038557733644999814, -10.11114377999000169, -317.5000000000000000 ) ) ;
#543 = EDGE_CURVE ( 'NONE', #1717, #2787, #7203, .T. ) ;
#544 = FACE_OUTER_BOUND ( 'NONE', #612, .T. ) ;
#545 = CARTESIAN_POINT ( 'NONE',  ( 13.92506561308973545, -5.424300063451886089, 315.0000000000000568 ) ) ;
#546 = CARTESIAN_POINT ( 'NONE',  ( -6.488017178959999853, 9.182784307579000327, -314.6383426456000052 ) ) ;
#547 = FACE_OUTER_BOUND ( 'NONE', #6635, .T. ) ;
#548 = CARTESIAN_POINT ( 'NONE',  ( 17.87038977196999312, 4.940238929760003117, 320.0770942683900557 ) ) ;
#549 = FILL_AREA_STYLE ('',( #8596 ) ) ;
#550 = CARTESIAN_POINT ( 'NONE',  ( -1.558284605000191947, -2.631303827346001878, -434.8033654657723446 ) ) ;
#551 = ORIENTED_EDGE ( 'NONE', *, *, #6050, .F. ) ;
#552 = CARTESIAN_POINT ( 'NONE',  ( -20.10152810630999554, 0.3450717431897997733, -317.0792622552969533 ) ) ;
#553 = CARTESIAN_POINT ( 'NONE',  ( -7.863726017345004315, -11.49810175465000661, -316.3802825947000201 ) ) ;
#554 = EDGE_CURVE ( 'NONE', #2675, #1542, #4062, .T. ) ;
#555 = CIRCLE ( 'NONE', #7588, 3.499999999999999556 ) ;
#556 = DIRECTION ( 'NONE',  ( -0.000000000000000000, 1.000000000000000000, 0.000000000000000000 ) ) ;
#557 = AXIS2_PLACEMENT_3D ( 'NONE', #8920, #6558, #7364 ) ;
#558 = CARTESIAN_POINT ( 'NONE',  ( -4.551150791544325003, 9.653623619670586464, -314.5171481538502576 ) ) ;
#559 =( REPRESENTATION_RELATIONSHIP ('NONE','NONE', #8468, #6273 ) REPRESENTATION_RELATIONSHIP_WITH_TRANSFORMATION ( #1777 )SHAPE_REPRESENTATION_RELATIONSHIP( ) );
#560 = ORIENTED_EDGE ( 'NONE', *, *, #8432, .T. ) ;
#561 = CARTESIAN_POINT ( 'NONE',  ( -17.80781204382000027, 3.997739559166000323, 190.0000000000000000 ) ) ;
#562 = CARTESIAN_POINT ( 'NONE',  ( 15.56166711177641204, -7.864757419948091410, 319.0000000000003979 ) ) ;
#563 = VERTEX_POINT ( 'NONE', #7338 ) ;
#564 = CARTESIAN_POINT ( 'NONE',  ( -14.00000000000000000, 2.500000000000000000, -380.4979246178999688 ) ) ;
#565 = ORIENTED_EDGE ( 'NONE', *, *, #5258, .F. ) ;
#566 = CARTESIAN_POINT ( 'NONE',  ( -4.780298404687055580, -9.113031460416761931, 315.0000000000000000 ) ) ;
#567 = CARTESIAN_POINT ( 'NONE',  ( -16.90094380520001849, -6.817658119454999444, -302.9207377450070453 ) ) ;
#568 = EDGE_CURVE ( 'NONE', #9067, #6664, #8056, .T. ) ;
#569 = FACE_OUTER_BOUND ( 'NONE', #2442, .T. ) ;
#570 = CIRCLE ( 'NONE', #6572, 15.50000000000002487 ) ;
#571 = CARTESIAN_POINT ( 'NONE',  ( -0.1153702471463786128, -7.665106240334001342, -434.0348060233743581 ) ) ;
#572 = CARTESIAN_POINT ( 'NONE',  ( -9.124390749379998056, 10.69353917616999539, -302.4229045757450081 ) ) ;
#573 = CARTESIAN_POINT ( 'NONE',  ( 17.61140045117998554, -5.929979699424000827, 318.8802828394900644 ) ) ;
#574 = VERTEX_POINT ( 'NONE', #5718 ) ;
#575 = CARTESIAN_POINT ( 'NONE',  ( -13.56771446467999986, -6.451120369226999607, -314.4150829855000211 ) ) ;
#576 = LINE ( 'NONE', #10569, #3520 ) ;
#577 = ORIENTED_EDGE ( 'NONE', *, *, #8567, .T. ) ;
#578 = CARTESIAN_POINT ( 'NONE',  ( -0.7033324871772000941, -12.09174782753000166, 189.9229057364800042 ) ) ;
#579 = CARTESIAN_POINT ( 'NONE',  ( -19.77468550638000266, 1.920668048511998904, 318.8802828394900644 ) ) ;
#580 = LINE ( 'NONE', #7938, #3620 ) ;
#581 = VECTOR ( 'NONE', #10244, 1000.000000000000000 ) ;
#582 = TOROIDAL_SURFACE ( 'NONE', #1960, 12.00000000000000000, 0.5000000000000000000 ) ;
#583 = ORIENTED_EDGE ( 'NONE', *, *, #4956, .T. ) ;
#584 = CARTESIAN_POINT ( 'NONE',  ( -13.31399140613000043, -6.082710156904999721, 314.8616023057000461 ) ) ;
#585 = DIRECTION ( 'NONE',  ( 0.000000000000000000, 1.000000000000000000, -0.000000000000000000 ) ) ;
#586 = CARTESIAN_POINT ( 'NONE',  ( -13.82226565756009684, 5.505830577453552088, 315.0000000000000568 ) ) ;
#587 = FACE_OUTER_BOUND ( 'NONE', #4840, .T. ) ;
#588 = CIRCLE ( 'NONE', #7964, 3.499999999999999556 ) ;
#589 = CARTESIAN_POINT ( 'NONE',  ( -3.970004819630974957, -9.235895690467337715, -315.0000000000000568 ) ) ;
#590 = CARTESIAN_POINT ( 'NONE',  ( 19.99999035944999903, -7.277437094418000096E-10, -303.5000000000000000 ) ) ;
#591 = CARTESIAN_POINT ( 'NONE',  ( -11.28781796570999951, 4.951468039558000633, 315.0000000000000000 ) ) ;
#592 = CIRCLE ( 'NONE', #7969, 4.000000000000009770 ) ;
#593 = ORIENTED_EDGE ( 'NONE', *, *, #693, .T. ) ;
#594 = DIRECTION ( 'NONE',  ( 0.000000000000000000, 1.000000000000000000, -0.000000000000000000 ) ) ;
#595 = AXIS2_PLACEMENT_3D ( 'NONE', #9903, #3452, #2538 ) ;
#596 = CARTESIAN_POINT ( 'NONE',  ( -4.780493465650554441, 9.113006550021843566, -314.9999999999999432 ) ) ;
#597 = EDGE_CURVE ( 'NONE', #10408, #168, #5818, .T. ) ;
#598 = CARTESIAN_POINT ( 'NONE',  ( 16.06942734036999454, 6.898991720969999797, 189.9229057364800042 ) ) ;
#599 = CARTESIAN_POINT ( 'NONE',  ( 17.50000000088856567, 5.867334121986925055, 190.0000000000002558 ) ) ;
#600 = CARTESIAN_POINT ( 'NONE',  ( -17.62191473184000046, -4.312542294520999242, -317.5000000000030127 ) ) ;
#601 = CIRCLE ( 'NONE', #6609, 3.500000000000006217 ) ;
#602 = CIRCLE ( 'NONE', #768, 0.5000000000000083267 ) ;
#603 = AXIS2_PLACEMENT_3D ( 'NONE', #7287, #4114, #782 ) ;
#604 = FACE_BOUND ( 'NONE', #4756, .T. ) ;
#605 = CARTESIAN_POINT ( 'NONE',  ( 323.0473732681808769, 4.999999999999984013, -355.4828474203333144 ) ) ;
#606 = CARTESIAN_POINT ( 'NONE',  ( -0.3764627761248945381, -12.50000000000000000, -361.1540620660322816 ) ) ;
#607 = CARTESIAN_POINT ( 'NONE',  ( 17.57772697299999720, -0.3191603157329999663, -314.4150829855000211 ) ) ;
#608 = FACE_OUTER_BOUND ( 'NONE', #8794, .T. ) ;
#609 = CARTESIAN_POINT ( 'NONE',  ( -11.81011838702999484, 9.634252844421009598, 320.0770942683900557 ) ) ;
#610 = DIRECTION ( 'NONE',  ( 1.000000000000000000, 0.000000000000000000, 0.000000000000000000 ) ) ;
#611 = CARTESIAN_POINT ( 'NONE',  ( -1.837389479601686304, -2.655393054924001461, -434.9057872931240354 ) ) ;
#612 = EDGE_LOOP ( 'NONE', ( #2471, #339, #8409, #673 ) ) ;
#613 = CARTESIAN_POINT ( 'NONE',  ( -19.56985579239002959, -0.3946094453810997660, -317.5770954168139610 ) ) ;
#614 = CARTESIAN_POINT ( 'NONE',  ( 11.75551710966999153, -10.11738730586000123, -316.3802825947000201 ) ) ;
#615 = FACE_OUTER_BOUND ( 'NONE', #9397, .T. ) ;
#616 = PRODUCT_RELATED_PRODUCT_CATEGORY ( 'part', '', ( #2183 ) ) ;
#617 = DIRECTION ( 'NONE',  ( -0.9396926207858973257, 0.000000000000000000, -0.3420201433256991330 ) ) ;
#618 = EDGE_LOOP ( 'NONE', ( #6699, #7554, #9225, #7750 ) ) ;
#619 = CARTESIAN_POINT ( 'NONE',  ( 19.99999721132999753, -3.518697978483000342E-10, 319.0000000000000000 ) ) ;
#620 = ORIENTED_EDGE ( 'NONE', *, *, #682, .T. ) ;
#621 = DIRECTION ( 'NONE',  ( -0.000000000000000000, 1.000000000000000000, 0.000000000000000000 ) ) ;
#622 = ORIENTED_EDGE ( 'NONE', *, *, #10050, .T. ) ;
#623 = CARTESIAN_POINT ( 'NONE',  ( -15.47214269673303200, -3.911151857093433382, 315.0000000000000568 ) ) ;
#624 = CARTESIAN_POINT ( 'NONE',  ( -19.95002954278003315, -1.762942793154997911, -302.9207377450070453 ) ) ;
#625 = CARTESIAN_POINT ( 'NONE',  ( 10.00000000000000000, 2.500000000000000000, -315.0000000000000000 ) ) ;
#626 = AXIS2_PLACEMENT_3D ( 'NONE', #8353, #8405, #4516 ) ;
#627 = ADVANCED_FACE ( 'NONE', ( #9915 ), #6187, .T. ) ;
#628 = CARTESIAN_POINT ( 'NONE',  ( 5.268482393219001025, 12.14948647186998976, -302.9207377450070453 ) ) ;
#629 = CARTESIAN_POINT ( 'NONE',  ( -5.273242226636224217, -7.500000000000000000, -350.0814130718403590 ) ) ;
#630 = EDGE_LOOP ( 'NONE', ( #9121, #1586 ) ) ;
#631 = CARTESIAN_POINT ( 'NONE',  ( 10.58688533405000065, -7.844683714540999553, -314.6383426456000052 ) ) ;
#632 = CARTESIAN_POINT ( 'NONE',  ( -17.13090252310000139, -0.3058267005333999977, 314.8616023057000461 ) ) ;
#633 = ORIENTED_EDGE ( 'NONE', *, *, #4237, .T. ) ;
#634 = CARTESIAN_POINT ( 'NONE',  ( 1.232798796115999851, -12.07489154382001040, 189.9229057364800042 ) ) ;
#635 = CARTESIAN_POINT ( 'NONE',  ( 9.974269275089660880, 10.84391064191637000, 190.9999999999996589 ) ) ;
#636 = CARTESIAN_POINT ( 'NONE',  ( -72.90663470096859555, -2.500000000000000000, -371.7168990827444190 ) ) ;
#637 = ADVANCED_FACE ( 'NONE', ( #3830 ), #4049, .F. ) ;
#638 = ORIENTED_EDGE ( 'NONE', *, *, #1595, .F. ) ;
#639 = CARTESIAN_POINT ( 'NONE',  ( -12.21495827233999876, -7.290170534263999969, 314.4150829855000211 ) ) ;
#640 = FACE_BOUND ( 'NONE', #5175, .T. ) ;
#641 = EDGE_CURVE ( 'NONE', #5506, #9376, #3255, .T. ) ;
#642 = CARTESIAN_POINT ( 'NONE',  ( 11.73784133842000088, 9.026952533543999735, 320.0000000000000000 ) ) ;
#643 = CARTESIAN_POINT ( 'NONE',  ( -1.281333103385001726, -11.37293729856000368, 319.9928079742500131 ) ) ;
#644 = CARTESIAN_POINT ( 'NONE',  ( 12.21612826667444729, 9.907025583609536667, 319.0000000000005116 ) ) ;
#645 = CARTESIAN_POINT ( 'NONE',  ( -17.50000000000000711, 8.653861160270983887E-10, 190.0000000000000568 ) ) ;
#646 = FACE_OUTER_BOUND ( 'NONE', #2355, .T. ) ;
#647 = ORIENTED_EDGE ( 'NONE', *, *, #4458, .T. ) ;
#648 = CARTESIAN_POINT ( 'NONE',  ( 10.23467948564923091, 9.999999999493891067, 190.0000000000002558 ) ) ;
#649 = CARTESIAN_POINT ( 'NONE',  ( -17.84297720825001221, 4.977647671642006166, 189.9229057364800042 ) ) ;
#650 = DIRECTION ( 'NONE',  ( -0.000000000000000000, 1.000000000000000000, 0.000000000000000000 ) ) ;
#651 = B_SPLINE_CURVE_WITH_KNOTS ( 'NONE', 3,
 ( #7741, #9568, #4623, #10319, #2960, #6230, #7896, #8699, #10222, #6077, #2857, #6178, #9366, #542, #3819, #7103, #2907, #8589, #9413, #4463, #5316, #9516, #1237, #2157, #10370, #2207, #9462, #439, #8754, #1397, #2102, #1293, #4680, #4513, #600, #6895, #2001, #7793, #5265 ),
 .UNSPECIFIED., .F., .F.,
 ( 4, 1, 1, 1, 1, 1, 1, 1, 1, 1, 1, 1, 1, 1, 1, 1, 1, 1, 1, 1, 1, 1, 1, 1, 1, 1, 1, 1, 1, 1, 1, 1, 1, 1, 1, 1, 4 ),
 ( 0.000000000000000000, 0.02777777777778000015, 0.05555555555556000030, 0.08333333333333001192, 0.1111111111111000027, 0.1388888888888999973, 0.1666666666667000196, 0.1944444444444000109, 0.2222222222222000054, 0.2500000000000000000, 0.2777777777777999946, 0.3055555555555999891, 0.3333333333333000081, 0.3611111111111000027, 0.3888888888888999973, 0.4166666666666999919, 0.4444444444444000109, 0.4722222222222000054, 0.5000000000000000000, 0.5277777777777999946, 0.5555555555555999891, 0.5833333333333000637, 0.6111111111111000582, 0.6388888888888999418, 0.6666666666667000474, 0.6944444444444000109, 0.7222222222222000054, 0.7500000000000000000, 0.7777777777777999946, 0.8055555555555999891, 0.8333333333333000637, 0.8611111111111000582, 0.8888888888888999418, 0.9166666666667000474, 0.9444444444444000109, 0.9722222222222000054, 1.000000000000000000 ),
 .UNSPECIFIED. ) ;
#652 = CIRCLE ( 'NONE', #5110, 12.50000000000002309 ) ;
#653 = FACE_OUTER_BOUND ( 'NONE', #7217, .T. ) ;
#654 = CARTESIAN_POINT ( 'NONE',  ( 11.77008734995756178, 6.834641529527616832, 315.0000000000000568 ) ) ;
#655 = ADVANCED_FACE ( 'NONE', ( #3024 ), #6350, .T. ) ;
#656 = APPLICATION_PROTOCOL_DEFINITION ( 'draft international standard', 'automotive_design', 1998, #9551 ) ;
#657 = FACE_OUTER_BOUND ( 'NONE', #6357, .T. ) ;
#658 = DIRECTION ( 'NONE',  ( -1.000000000000000000, 0.000000000000000000, 0.000000000000000000 ) ) ;
#659 = CARTESIAN_POINT ( 'NONE',  ( -18.86319819242002183, -0.4765179085981003926, 319.9928079742500131 ) ) ;
#660 = CARTESIAN_POINT ( 'NONE',  ( -1.444632214126728043, -2.659134901855999988, -434.9867182716628236 ) ) ;
#661 = VERTEX_POINT ( 'NONE', #3239 ) ;
#662 = CARTESIAN_POINT ( 'NONE',  ( -6.769722431736004076, 11.85293133419998846, -317.0792622552969533 ) ) ;
#663 = CARTESIAN_POINT ( 'NONE',  ( 3.762811461229003562, -12.28417267642999278, -316.3802825947000201 ) ) ;
#664 = ORIENTED_EDGE ( 'NONE', *, *, #4434, .T. ) ;
#665 = CARTESIAN_POINT ( 'NONE',  ( -79.31727611502927289, -2.500000000000000000, -351.2304352734219606 ) ) ;
#666 = B_SPLINE_CURVE_WITH_KNOTS ( 'NONE', 3,
 ( #4430, #5384, #5329, #349, #4384, #10335, #8456, #2766, #4475, #7755, #9429, #3676, #8664, #1097, #6963, #10237, #6038, #9328, #1964, #6909, #2873, #8605, #1251, #3728, #10285, #2924, #558, #4860, #7225, #8886, #8939, #7169, #3079, #8832, #8715, #9530, #2388, #2224, #7331, #10439, #4055, #7912, #5493, #3890, #2170, #9748 ),
 .UNSPECIFIED., .F., .F.,
 ( 4, 2, 2, 2, 2, 2, 2, 2, 2, 2, 2, 2, 2, 2, 2, 2, 2, 2, 2, 2, 2, 2, 4 ),
 ( 0.000000000000000000, 0.001362852592701295929, 0.002044278889051944111, 0.002725705185402593159, 0.004088557778103887354, 0.005451410370805182849, 0.006814262963506478345, 0.008177115556207774708, 0.01090282074161036743, 0.01635423111241555982, 0.01907993629781816122, 0.02180564148322075915, 0.02453134666862336055, 0.02725705185402596195, 0.02998275703942856335, 0.03270846222483116128, 0.03543416741023376615, 0.03815987259563636408, 0.03952272518833765264, 0.04088557778103895507, 0.04224843037374024363, 0.04292985667009089484, 0.04361128296644153912 ),
 .UNSPECIFIED. ) ;
#667 = PRODUCT_DEFINITION_CONTEXT ( 'detailed design', #7443, 'design' ) ;
#668 = LINE ( 'NONE', #3943, #1019 ) ;
#669 = CARTESIAN_POINT ( 'NONE',  ( 16.99996037728000076, -1.352915083302999933E-09, -314.9999801883000146 ) ) ;
#670 = EDGE_CURVE ( 'NONE', #1738, #2124, #8074, .T. ) ;
#671 = ORIENTED_EDGE ( 'NONE', *, *, #1195, .T. ) ;
#672 = CARTESIAN_POINT ( 'NONE',  ( 10.97430844189483423, -10.45950866754415820, 319.0000000000003979 ) ) ;
#673 = ORIENTED_EDGE ( 'NONE', *, *, #1413, .T. ) ;
#674 = CARTESIAN_POINT ( 'NONE',  ( 13.89291764776418603, 9.007512922137015821, -316.5000000000004547 ) ) ;
#675 = ORIENTED_EDGE ( 'NONE', *, *, #9162, .F. ) ;
#676 = CARTESIAN_POINT ( 'NONE',  ( -5.241997271368903810, -9.033710068163633977, 315.0000000000000000 ) ) ;
#677 = CARTESIAN_POINT ( 'NONE',  ( -20.06799914428001941, 0.4075895895062001673, -302.9207377450070453 ) ) ;
#678 = DIRECTION ( 'NONE',  ( 0.000000000000000000, 1.000000000000000000, 0.000000000000000000 ) ) ;
#679 = DIRECTION ( 'NONE',  ( -0.9554399839384175586, 0.000000000000000000, -0.2951854283188048989 ) ) ;
#680 = VECTOR ( 'NONE', #1083, 1000.000000000000000 ) ;
#681 = CIRCLE ( 'NONE', #10112, 3.499999999999997335 ) ;
#682 = EDGE_CURVE ( 'NONE', #9376, #10131, #2383, .T. ) ;
#683 = CARTESIAN_POINT ( 'NONE',  ( -5.058393412147005108, 12.18538300202998315, -302.9207377450070453 ) ) ;
#684 = CARTESIAN_POINT ( 'NONE',  ( -12.21300849950000433, -9.900542285453001412, 318.8802828394900644 ) ) ;
#685 = ORIENTED_EDGE ( 'NONE', *, *, #8921, .F. ) ;
#686 = CARTESIAN_POINT ( 'NONE',  ( 13.62823431091000081, -6.408810695481999886, -314.4150829855000211 ) ) ;
#687 = CARTESIAN_POINT ( 'NONE',  ( -2.000000000000000000, -9.500000000000000000, -404.4999999999999432 ) ) ;
#688 = EDGE_LOOP ( 'NONE', ( #10453, #7051, #5685, #108 ) ) ;
#689 = CARTESIAN_POINT ( 'NONE',  ( 16.06649953495000105, -6.900914778667005756, 189.9229057364800042 ) ) ;
#690 = CARTESIAN_POINT ( 'NONE',  ( -13.10504385913262837, 9.452822371482907826, 190.9999999999996589 ) ) ;
#691 = CARTESIAN_POINT ( 'NONE',  ( -1002.398135702230206, -7.500000000000000000, -618.0215964952759577 ) ) ;
#692 = AXIS2_PLACEMENT_3D ( 'NONE', #6618, #5963, #1017 ) ;
#693 = EDGE_CURVE ( 'NONE', #3804, #8252, #9594, .T. ) ;
#694 = EDGE_CURVE ( 'NONE', #9461, #7519, #8991, .T. ) ;
#695 = CARTESIAN_POINT ( 'NONE',  ( 1.388768300183999882, -9.421618921053999784, 315.0848619657999734 ) ) ;
#696 = CYLINDRICAL_SURFACE ( 'NONE', #389, 1.999999999999980238 ) ;
#697 = FACE_OUTER_BOUND ( 'NONE', #8610, .T. ) ;
#698 = PRESENTATION_STYLE_ASSIGNMENT (( #6324 ) ) ;
#699 = DIRECTION ( 'NONE',  ( 0.000000000000000000, -1.000000000000000000, 0.000000000000000000 ) ) ;
#700 = VERTEX_POINT ( 'NONE', #818 ) ;
#701 = CARTESIAN_POINT ( 'NONE',  ( 1.279515965483999906E-07, 10.00000000755999885, 190.0000000000000000 ) ) ;
#702 = CARTESIAN_POINT ( 'NONE',  ( -4.791123986588002204, 11.72534684832999119, 189.9229057364800042 ) ) ;
#703 = DIRECTION ( 'NONE',  ( -0.4712473909295803454, 0.000000000000000000, 0.8820010751365688906 ) ) ;
#704 = EDGE_CURVE ( 'NONE', #8266, #7812, #5649, .T. ) ;
#705 = DIRECTION ( 'NONE',  ( -0.9712267471052612455, 0.000000000000000000, -0.2381566831044910626 ) ) ;
#706 =( BOUNDED_SURFACE ( )  B_SPLINE_SURFACE ( 3, 1, ( 
 ( #9973, #6695 ),
 ( #7344, #9011 ),
 ( #5876, #1646 ),
 ( #9168, #7446 ),
 ( #32, #10026 ),
 ( #2508, #6588 ),
 ( #4922, #8198 ) ),
 .UNSPECIFIED., .F., .F., .F. ) 
 B_SPLINE_SURFACE_WITH_KNOTS ( ( 4, 3, 4 ),
 ( 2, 2 ),
 ( 0.000000000000000000, 0.5000000000000000000, 1.000000000000000000 ),
 ( 0.000000000000000000, 1.000000000000000000 ),
 .UNSPECIFIED. ) 
 GEOMETRIC_REPRESENTATION_ITEM ( )  RATIONAL_B_SPLINE_SURFACE ( (
 ( 1.000000000000000000, 1.000000000000000000),
 ( 0.8047378516590519837, 0.8047378516590519837),
 ( 0.8047378516590519837, 0.8047378516590519837),
 ( 1.000000000000000000, 1.000000000000000000),
 ( 0.8047378516590519837, 0.8047378516590519837),
 ( 0.8047378516590519837, 0.8047378516590519837),
 ( 1.000000000000000000, 1.000000000000000000) ) ) 
 REPRESENTATION_ITEM ( '' )  SURFACE ( )  );
#707 = CARTESIAN_POINT ( 'NONE',  ( 17.49999999954662044, -9.625715914672042649E-06, 190.0000000000000000 ) ) ;
#708 = SHAPE_DEFINITION_REPRESENTATION ( #7165, #4020 ) ;
#709 = CARTESIAN_POINT ( 'NONE',  ( -119.6503683519543983, -2.500000000000000000, -299.0840866897705155 ) ) ;
#710 = CARTESIAN_POINT ( 'NONE',  ( 16.98808798087999961, 1.334629195702000004, -314.8616023057000461 ) ) ;
#711 = DIRECTION ( 'NONE',  ( 0.000000000000000000, -1.000000000000000000, 0.000000000000000000 ) ) ;
#712 = CARTESIAN_POINT ( 'NONE',  ( -19.37251270682998694, 1.820313540576997680, 320.0770942683900557 ) ) ;
#713 =( LENGTH_UNIT ( ) NAMED_UNIT ( * ) SI_UNIT ( .MILLI., .METRE. ) );
#714 = CARTESIAN_POINT ( 'NONE',  ( -0.5380925645899466980, -2.513321162497997197, -434.0383604270527940 ) ) ;
#715 = ORIENTED_EDGE ( 'NONE', *, *, #7705, .F. ) ;
#716 = CARTESIAN_POINT ( 'NONE',  ( 18.19038122738000141, 4.511441183124001775, -317.5770954168139610 ) ) ;
#717 = CARTESIAN_POINT ( 'NONE',  ( 18.56065892533998962, -4.703159488203003669, -316.3802825947000201 ) ) ;
#718 = CARTESIAN_POINT ( 'NONE',  ( -18.53598399141000286, -2.541378258162000137, 320.0000000000000000 ) ) ;
#719 = AXIS2_PLACEMENT_3D ( 'NONE', #5470, #4675, #10264 ) ;
#720 = FACE_BOUND ( 'NONE', #6913, .T. ) ;
#721 = CARTESIAN_POINT ( 'NONE',  ( 16.53772850381890791, -2.187491735906823997, -314.9999999999998863 ) ) ;
#722 = VERTEX_POINT ( 'NONE', #8182 ) ;
#723 = DIRECTION ( 'NONE',  ( 0.9848077530122130163, 0.000000000000000000, 0.1736481776669025201 ) ) ;
#724 = ORIENTED_EDGE ( 'NONE', *, *, #7423, .T. ) ;
#725 = CARTESIAN_POINT ( 'NONE',  ( 15.92495094281444601, 7.583842622554345603, -316.5000000000004547 ) ) ;
#726 = VERTEX_POINT ( 'NONE', #7376 ) ;
#727 =( BOUNDED_CURVE ( )  B_SPLINE_CURVE ( 3, ( #4537, #2178, #9337, #3788, #7716, #7022, #2073 ),
 .UNSPECIFIED., .F., .T. ) 
 B_SPLINE_CURVE_WITH_KNOTS ( ( 4, 3, 4 ),
 ( 0.006576891565977574343, 0.5000000000000000000, 0.9934231084340225948 ),
 .UNSPECIFIED. ) 
 CURVE ( )  GEOMETRIC_REPRESENTATION_ITEM ( )  RATIONAL_B_SPLINE_CURVE ( ( 0.9922222087809801083, 0.8003084355045907428, 0.8029010325775972623, 1.000000000000000000, 0.8029010325775971513, 0.8003084355045906317, 0.9922222087809804414 ) ) 
 REPRESENTATION_ITEM ( '' )  );
#728 = CARTESIAN_POINT ( 'NONE',  ( -14.89844356947526727, -4.564575774521109963, 315.0000000000000000 ) ) ;
#729 = CARTESIAN_POINT ( 'NONE',  ( 4.978480136836995307, -11.69377972944999478, -302.4229045757450081 ) ) ;
#730 = DIRECTION ( 'NONE',  ( 0.4712473909295803454, 0.000000000000000000, -0.8820010751365688906 ) ) ;
#731 = VECTOR ( 'NONE', #6902, 1000.000000000000000 ) ;
#732 = VECTOR ( 'NONE', #8909, 1000.000000000000000 ) ;
#733 = CARTESIAN_POINT ( 'NONE',  ( 9.378959784071181360, -5.899999999999999467, -525.1866552614185366 ) ) ;
#734 = CARTESIAN_POINT ( 'NONE',  ( -1.652129430310999236, 12.05325387113999014, -302.4229045757450081 ) ) ;
#735 = CARTESIAN_POINT ( 'NONE',  ( 19.98389199037000452, 0.4027620370101000491, 318.8802828394900644 ) ) ;
#736 = ORIENTED_EDGE ( 'NONE', *, *, #7510, .T. ) ;
#737 = CARTESIAN_POINT ( 'NONE',  ( 10.49789511286000021, -7.639556387670999982, -314.8616023057000461 ) ) ;
#738 = CARTESIAN_POINT ( 'NONE',  ( -17.57673583306999632, -0.3313182897943000582, 314.4150829855000211 ) ) ;
#739 = EDGE_LOOP ( 'NONE', ( #961, #10607, #7941, #3569 ) ) ;
#740 = CARTESIAN_POINT ( 'NONE',  ( 4.791123986588002204, -11.72534684832999119, 189.9229057364800042 ) ) ;
#741 = CARTESIAN_POINT ( 'NONE',  ( -19.78120799650142558, 1.924098540961039605, 190.9999999999996589 ) ) ;
#742 = DIRECTION ( 'NONE',  ( 1.000000000000000000, 0.000000000000000000, 0.000000000000000000 ) ) ;
#743 = CARTESIAN_POINT ( 'NONE',  ( 1.399029207469000058, -9.644928263551999947, 314.8616023057000461 ) ) ;
#744 = CARTESIAN_POINT ( 'NONE',  ( -18.95675155274000190, 0.9190877154199000865, 320.0000000000000000 ) ) ;
#745 = DIRECTION ( 'NONE',  ( 0.000000000000000000, 1.000000000000000000, -0.000000000000000000 ) ) ;
#746 = CARTESIAN_POINT ( 'NONE',  ( 18.71196753105320099, 4.439097376277246099, 319.0000000000005116 ) ) ;
#747 = DIRECTION ( 'NONE',  ( 0.000000000000000000, 0.000000000000000000, 1.000000000000000000 ) ) ;
#748 = EDGE_LOOP ( 'NONE', ( #1545, #9667, #1018, #6857 ) ) ;
#749 = CARTESIAN_POINT ( 'NONE',  ( -11.71572875797656188, 12.49999999864037825, -303.5000000000000000 ) ) ;
#750 = ORIENTED_EDGE ( 'NONE', *, *, #4566, .F. ) ;
#751 = ORIENTED_EDGE ( 'NONE', *, *, #437, .F. ) ;
#752 = CARTESIAN_POINT ( 'NONE',  ( -1.999999999997229772, -7.500000000000000000, -409.4999999999571969 ) ) ;
#753 = CARTESIAN_POINT ( 'NONE',  ( 14.08994485310920730, 5.290256584484003710, 314.9999999999999432 ) ) ;
#754 = VECTOR ( 'NONE', #1389, 1000.000000000000227 ) ;
#755 = CARTESIAN_POINT ( 'NONE',  ( -11.70471109486296690, -10.14826236475114740, -303.4999999999996589 ) ) ;
#756 = CARTESIAN_POINT ( 'NONE',  ( 16.19514236092000203, 2.730451569713999938, -315.0848619657999734 ) ) ;
#757 = EDGE_CURVE ( 'NONE', #9634, #5121, #13, .T. ) ;
#758 = DIRECTION ( 'NONE',  ( -1.000000000000000000, 0.000000000000000000, 0.000000000000000000 ) ) ;
#759 = CARTESIAN_POINT ( 'NONE',  ( -3.656057816511529168, -7.040919069177174805, -436.0988728614874503 ) ) ;
#760 = CARTESIAN_POINT ( 'NONE',  ( 17.64852322130001738, 5.886271888320000478, 318.8802828394900644 ) ) ;
#761 = CARTESIAN_POINT ( 'NONE',  ( 10.00000000000000000, 2.500000000000000000, -285.0000000000000000 ) ) ;
#762 = EDGE_CURVE ( 'NONE', #7526, #1962, #7547, .T. ) ;
#763 = CARTESIAN_POINT ( 'NONE',  ( 7.006889269069000115, 6.844138725329000472, -284.9999999999999432 ) ) ;
#764 = ORIENTED_EDGE ( 'NONE', *, *, #7485, .F. ) ;
#765 = CARTESIAN_POINT ( 'NONE',  ( 19.86719273998999213, 1.743644188460999667, -316.3802825947000201 ) ) ;
#766 = CARTESIAN_POINT ( 'NONE',  ( -19.98383894087000812, 0.4026063077914996402, -316.3802825947000201 ) ) ;
#767 = AXIS2_PLACEMENT_3D ( 'NONE', #8861, #5631, #3922 ) ;
#768 = AXIS2_PLACEMENT_3D ( 'NONE', #2666, #7549, #1150 ) ;
#769 = CARTESIAN_POINT ( 'NONE',  ( -18.78897325516000194, -1.756194273835000041, 320.0000000000000000 ) ) ;
#770 = EDGE_CURVE ( 'NONE', #2618, #5251, #7738, .T. ) ;
#771 = CARTESIAN_POINT ( 'NONE',  ( -1.000888714456147133, -7.421678258158998176, -434.5721179219322039 ) ) ;
#772 = UNCERTAINTY_MEASURE_WITH_UNIT (LENGTH_MEASURE( 1.000000000000000082E-05 ), #971, 'distance_accuracy_value', 'NONE');
#773 = DIRECTION ( 'NONE',  ( 0.000000000000000000, 1.000000000000000000, -0.000000000000000000 ) ) ;
#774 = DIRECTION ( 'NONE',  ( 0.000000000000000000, -1.000000000000000000, 0.000000000000000000 ) ) ;
#776 = ORIENTED_EDGE ( 'NONE', *, *, #694, .F. ) ;
#775 = AXIS2_PLACEMENT_3D ( 'NONE', #6193, #1570, #9735 ) ;
#777 = FACE_OUTER_BOUND ( 'NONE', #6314, .T. ) ;
#778 = ORIENTED_EDGE ( 'NONE', *, *, #2712, .F. ) ;
#779 = CARTESIAN_POINT ( 'NONE',  ( -5.323201728285183343, 12.06184864676790269, -316.5000000000004547 ) ) ;
#780 = EDGE_LOOP ( 'NONE', ( #4389, #3578, #5980, #685 ) ) ;
#781 = CARTESIAN_POINT ( 'NONE',  ( 19.97270637197000909, 0.5553832019671997022, -303.6197174156509391 ) ) ;
#782 = DIRECTION ( 'NONE',  ( 0.000000000000000000, 0.000000000000000000, -1.000000000000000000 ) ) ;
#783 = DIRECTION ( 'NONE',  ( 0.000000000000000000, -1.000000000000000000, 0.000000000000000000 ) ) ;
#784 = STYLED_ITEM ( 'NONE', ( #5890 ), #966 ) ;
#785 = CARTESIAN_POINT ( 'NONE',  ( 5.185096592093999313, 11.65847420015999170, -302.4229045757450081 ) ) ;
#786 = EDGE_CURVE ( 'NONE', #1407, #3834, #1784, .T. ) ;
#787 = CARTESIAN_POINT ( 'NONE',  ( -38.85901494634669007, -12.00000000000000000, -386.6556615250812570 ) ) ;
#788 = ORIENTED_EDGE ( 'NONE', *, *, #10618, .F. ) ;
#789 = FACE_OUTER_BOUND ( 'NONE', #10203, .T. ) ;
#790 = CARTESIAN_POINT ( 'NONE',  ( -2.272356604769890431, -2.599354866276060605, -434.9211891149597591 ) ) ;
#791 = ORIENTED_EDGE ( 'NONE', *, *, #4315, .T. ) ;
#792 = CARTESIAN_POINT ( 'NONE',  ( -16.79769345205001585, -5.168336178625003718, 190.0071920248299477 ) ) ;
#793 = CARTESIAN_POINT ( 'NONE',  ( 11.03108320835583633, 10.43614982842405858, 190.9999999999996589 ) ) ;
#794 = CARTESIAN_POINT ( 'NONE',  ( 8.096765587028130540, 8.344222180821057933, -315.0000000000000000 ) ) ;
#795 = CARTESIAN_POINT ( 'NONE',  ( -72.90663470096859555, -2.500000000000000000, -371.7168990827444190 ) ) ;
#796 = VECTOR ( 'NONE', #10114, 1000.000000000000000 ) ;
#797 = CARTESIAN_POINT ( 'NONE',  ( -16.89608781496000134, -0.5923740909019999945, 315.0848619657999734 ) ) ;
#798 = CARTESIAN_POINT ( 'NONE',  ( 17.81405818021000087, 3.987619665940000502, 320.0000000000000000 ) ) ;
#799 = CARTESIAN_POINT ( 'NONE',  ( -18.89057790499001754, -0.06397434778252995835, 319.9928079742500131 ) ) ;
#800 = CARTESIAN_POINT ( 'NONE',  ( 14.88027513490714249, 8.363422937417032799, 319.0000000000005116 ) ) ;
#801 = DIRECTION ( 'NONE',  ( -0.9942380540931650135, 0.000000000000000000, -0.1071946444232960011 ) ) ;
#802 = CARTESIAN_POINT ( 'NONE',  ( -14.79012398733999945, 1.483731117707000058, 315.0000000000000000 ) ) ;
#803 = ORIENTED_EDGE ( 'NONE', *, *, #2276, .T. ) ;
#804 = VECTOR ( 'NONE', #5315, 1000.000000000000114 ) ;
#805 = DIRECTION ( 'NONE',  ( -0.9712267471052594692, 0.000000000000000000, -0.2381566831044984178 ) ) ;
#806 = CARTESIAN_POINT ( 'NONE',  ( 14.89844356947526727, 4.564575774521109963, 315.0000000000000000 ) ) ;
#807 = CARTESIAN_POINT ( 'NONE',  ( -98.44423576012317767, -2.500000000000000000, -338.7741350709160315 ) ) ;
#808 = CARTESIAN_POINT ( 'NONE',  ( 17.34710322845000263, -0.4172063223308000168, -314.6383426456000052 ) ) ;
#809 = DIRECTION ( 'NONE',  ( 0.000000000000000000, 1.000000000000000000, 0.000000000000000000 ) ) ;
#810 = EDGE_CURVE ( 'NONE', #8301, #3853, #10500, .T. ) ;
#811 = B_SPLINE_CURVE_WITH_KNOTS ( 'NONE', 3,
 ( #7075, #6916, #7815, #461, #3585, #10343, #6865, #2832, #1158, #6101, #10294, #2931, #6199, #4704, #6306, #8085, #623, #9590, #9644, #6363, #728, #2286, #4004, #3144, #2394, #8723, #5551, #6417, #5610, #4649, #8778, #2232, #5660, #7231, #7983, #8839, #7126, #10445, #1483, #3842, #7919, #4761, #7284, #8031, #3897, #1421, #8945, #9701, #3086, #7176, #676, #5499, #566, #3951, #2341, #4814, #10498, #10393, #8892, #1531, #10560, #3033, #3200, #6472, #9754, #1589, #1366, #6130, #7796, #2105, #442, #7003, #8702, #6951, #1241, #1186, #1346, #5480, #6080, #7744, #8759, #7057, #7694, #387, #10321, #2963, #9571, #10275, #496, #1400, #2004, #4628, #3661, #6234, #5371, #3615, #2860, #2807, #9370, #10225, #5318, #9417, #7900, #545, #5268, #6897, #337, #2053, #3821, #9464, #7106, #9521, #8543, #8592, #4465, #10375, #4517, #3717, #10164, #2912, #3015, #6180, #8652, #6289, #1295, #2211, #4575, #7849, #3764, #2160, #5426, #4558, #6437 ),
 .UNSPECIFIED., .F., .F.,
 ( 4, 1, 1, 1, 1, 1, 2, 2, 1, 1, 1, 1, 1, 2, 2, 1, 1, 1, 1, 1, 2, 2, 1, 1, 1, 1, 1, 2, 2, 1, 1, 1, 1, 1, 1, 2, 2, 1, 1, 1, 1, 1, 2, 2, 1, 1, 2, 2, 2, 1, 1, 2, 2, 1, 1, 1, 1, 2, 2, 1, 1, 1, 1, 1, 1, 2, 2, 1, 1, 1, 1, 1, 2, 2, 1, 1, 1, 1, 1, 2, 2, 1, 1, 1, 1, 1, 2, 2, 1, 1, 1, 1, 2, 2, 1, 1, 1, 2, 2, 4 ),
 ( 0.000000000000000000, 0.06250000000000791034, 0.09375000000001181000, 0.1093750000000137529, 0.1171875000000147105, 0.1210937500000152794, 0.1230468750000155709, 0.1250000000000158484, 0.1562500000000223432, 0.1718750000000255906, 0.1796875000000270617, 0.1835937500000277833, 0.1855468750000281719, 0.1865234375000283107, 0.1875000000000284217, 0.2187500000000311418, 0.2343750000000323908, 0.2421875000000330014, 0.2460937500000334177, 0.2480468750000336398, 0.2490234375000336953, 0.2500000000000337508, 0.2812500000000370259, 0.2968750000000386358, 0.3046875000000394684, 0.3085937500000398570, 0.3105468750000400235, 0.3115234375000401346, 0.3125000000000403011, 0.3437500000000445199, 0.3593750000000465739, 0.3671875000000476286, 0.3710937500000481282, 0.3730468750000484057, 0.3740234375000484612, 0.3745117187500484612, 0.3750000000000484612, 0.4062500000000490163, 0.4218750000000493494, 0.4296875000000495159, 0.4335937500000495715, 0.4355468750000495715, 0.4365234375000495715, 0.4375000000000495715, 0.4531250000000494604, 0.4609375000000494049, 0.4648437500000494049, 0.4687500000000494049, 0.5000000000000491829, 0.5156250000000491829, 0.5234375000000491829, 0.5273437500000490719, 0.5312500000000490719, 0.5468750000000488498, 0.5546875000000488498, 0.5585937500000488498, 0.5605468750000488498, 0.5615234375000488498, 0.5625000000000488498, 0.5937500000000481837, 0.6093750000000478506, 0.6171875000000476286, 0.6210937500000475175, 0.6230468750000474065, 0.6240234375000474065, 0.6245117187500474065, 0.6250000000000472955, 0.6562500000000430767, 0.6718750000000409672, 0.6796875000000398570, 0.6835937500000393019, 0.6855468750000390799, 0.6865234375000389688, 0.6875000000000388578, 0.7187500000000363043, 0.7343750000000350830, 0.7421875000000345279, 0.7460937500000343059, 0.7480468750000340838, 0.7490234375000340838, 0.7500000000000340838, 0.7812500000000317524, 0.7968750000000304201, 0.8046875000000298650, 0.8085937500000295319, 0.8105468750000293099, 0.8115234375000293099, 0.8125000000000293099, 0.8437500000000242029, 0.8593750000000216493, 0.8671875000000203171, 0.8710937500000196509, 0.8730468750000193179, 0.8750000000000189848, 0.9062500000000143219, 0.9218750000000121014, 0.9296875000000109912, 0.9335937500000103251, 0.9375000000000097700, 1.000000000000000000 ),
 .UNSPECIFIED. ) ;
#812 = CARTESIAN_POINT ( 'NONE',  ( -76.33371517498638070, -2.500000000000000000, -329.2281998388791635 ) ) ;
#813 = DIRECTION ( 'NONE',  ( 0.000000000000000000, 0.000000000000000000, 1.000000000000000000 ) ) ;
#814 = DIRECTION ( 'NONE',  ( -0.4716280258120419955, 0.000000000000000000, 0.8817975988108811558 ) ) ;
#815 = CARTESIAN_POINT ( 'NONE',  ( -15.03660170392436335, -3.530928676948000167, -439.4670019462156461 ) ) ;
#816 = VECTOR ( 'NONE', #6829, 1000.000000000000000 ) ;
#817 = CARTESIAN_POINT ( 'NONE',  ( 13.93268562690000678, 9.073621533052996568, -317.0792622552969533 ) ) ;
#818 = CARTESIAN_POINT ( 'NONE',  ( -87.43749534091338660, -2.500000000000000000, -367.8627987905216514 ) ) ;
#819 = ADVANCED_FACE ( 'NONE', ( #8387 ), #3450, .T. ) ;
#820 = CARTESIAN_POINT ( 'NONE',  ( -14.99960151356000004, -7.033824075090999273, 320.0000000000000000 ) ) ;
#821 = EDGE_CURVE ( 'NONE', #2499, #5421, #2800, .T. ) ;
#822 = CARTESIAN_POINT ( 'NONE',  ( -0.3462645226701464574, -7.523938431909999558, -434.3437067901672322 ) ) ;
#823 = CIRCLE ( 'NONE', #4941, 0.5000000000000128786 ) ;
#824 = CARTESIAN_POINT ( 'NONE',  ( -0.6228901166779408083, -2.499999376604999934, -434.1632067468180480 ) ) ;
#825 = CARTESIAN_POINT ( 'NONE',  ( 8.900723324022980165, -8.081813809772741664, -315.0000000000000000 ) ) ;
#826 = EDGE_LOOP ( 'NONE', ( #4070, #3945, #7397, #4001, #5011, #9817, #8400, #8877 ) ) ;
#827 = CARTESIAN_POINT ( 'NONE',  ( 12.98706127646999953, 6.788989183774999603, -314.4963898845653603 ) ) ;
#828 = ORIENTED_EDGE ( 'NONE', *, *, #8175, .T. ) ;
#829 = CARTESIAN_POINT ( 'NONE',  ( -13.36995595564000006, 8.154012700520999246, -317.5000000000000000 ) ) ;
#830 = VERTEX_POINT ( 'NONE', #9310 ) ;
#831 = DIRECTION ( 'NONE',  ( 0.000000000000000000, -1.000000000000000000, 0.000000000000000000 ) ) ;
#832 = DIRECTION ( 'NONE',  ( -0.5969176327498910695, 0.000000000000000000, -0.8023025238102309276 ) ) ;
#833 = EDGE_CURVE ( 'NONE', #245, #7676, #3711, .T. ) ;
#834 = CARTESIAN_POINT ( 'NONE',  ( -15.00000000000000000, -0.4945770392355999800, 315.0000000000000000 ) ) ;
#835 = CARTESIAN_POINT ( 'NONE',  ( -16.93986923087000562, 6.779672025222003739, -302.9207377450070453 ) ) ;
#836 = DIRECTION ( 'NONE',  ( 0.000000000000000000, 1.000000000000000000, 0.000000000000000000 ) ) ;
#837 = ORIENTED_EDGE ( 'NONE', *, *, #2330, .F. ) ;
#838 = DIRECTION ( 'NONE',  ( 1.000000000000000000, 0.000000000000000000, 0.000000000000000000 ) ) ;
#839 = DIRECTION ( 'NONE',  ( -0.000000000000000000, 1.000000000000000000, 0.000000000000000000 ) ) ;
#840 = ORIENTED_EDGE ( 'NONE', *, *, #770, .T. ) ;
#841 = CARTESIAN_POINT ( 'NONE',  ( -19.56991616969001058, 0.3941640562313002416, 189.9229057364800042 ) ) ;
#842 = CARTESIAN_POINT ( 'NONE',  ( -13.99679147458261319, 8.939383429014137405, 190.9999999999996589 ) ) ;
#843 = CARTESIAN_POINT ( 'NONE',  ( 11.72583169940718584, 6.858410958448125427, -315.0000000000000000 ) ) ;
#844 = CARTESIAN_POINT ( 'NONE',  ( -27.92645732311833129, -8.000000000000000000, -417.8271580078820762 ) ) ;
#845 = AXIS2_PLACEMENT_3D ( 'NONE', #2139, #530, #7882 ) ;
#846 = CARTESIAN_POINT ( 'NONE',  ( 13.37260572687999982, -6.041714840053000302, 314.8616023057000461 ) ) ;
#847 = CARTESIAN_POINT ( 'NONE',  ( 6.294482982547999761, 10.85527983184999989, 320.0000000000000000 ) ) ;
#848 = CARTESIAN_POINT ( 'NONE',  ( 16.03176714517000079, -6.932210726315004123, 320.0770942683900557 ) ) ;
#849 = CARTESIAN_POINT ( 'NONE',  ( -19.95988936745280995, 0.9706423173584770581, 319.0000000000005116 ) ) ;
#850 = CARTESIAN_POINT ( 'NONE',  ( 16.84717009645851604, 6.762270094121639374, -303.4999999999990905 ) ) ;
#851 = CARTESIAN_POINT ( 'NONE',  ( 11.99990625867999938, 6.898016740823000426, 314.8616023057000461 ) ) ;
#852 = ORIENTED_EDGE ( 'NONE', *, *, #3700, .T. ) ;
#853 = CARTESIAN_POINT ( 'NONE',  ( 4.000000000000000000, -2.500000000000000000, -410.4979246179000256 ) ) ;
#854 = ORIENTED_EDGE ( 'NONE', *, *, #8756, .F. ) ;
#855 = AXIS2_PLACEMENT_3D ( 'NONE', #8187, #8233, #7224 ) ;
#856 = CARTESIAN_POINT ( 'NONE',  ( -13.22841709878402483, -6.750000000003000267, -437.9939892205655383 ) ) ;
#857 = AXIS2_PLACEMENT_3D ( 'NONE', #198, #4972, #8247 ) ;
#858 = CARTESIAN_POINT ( 'NONE',  ( 13.64105609808563457, 5.653588212731087026, 315.0000000000000000 ) ) ;
#859 = CONTEXT_DEPENDENT_SHAPE_REPRESENTATION ( #10103, #8021 ) ;
#860 = CARTESIAN_POINT ( 'NONE',  ( -37.82921798586427542, -8.000000000000000000, -422.3602549205905916 ) ) ;
#861 = DIRECTION ( 'NONE',  ( 0.000000000000000000, 1.000000000000000000, 0.000000000000000000 ) ) ;
#862 = DIRECTION ( 'NONE',  ( 0.8820010751365675583, 0.000000000000000000, 0.4712473909295827323 ) ) ;
#863 = VERTEX_POINT ( 'NONE', #6651 ) ;
#864 = CARTESIAN_POINT ( 'NONE',  ( 10.49155472272000011, 10.73755170802999714, -317.0792622552969533 ) ) ;
#865 = VECTOR ( 'NONE', #3827, 1000.000000000000000 ) ;
#866 = PRESENTATION_LAYER_ASSIGNMENT (  '', '', ( #531 ) ) ;
#867 = EDGE_CURVE ( 'NONE', #9012, #3885, #7657, .T. ) ;
#868 = CARTESIAN_POINT ( 'NONE',  ( 16.83239583074999857, -5.311267823799999732, 320.0000000000000000 ) ) ;
#869 = CARTESIAN_POINT ( 'NONE',  ( -1.322461528884503412, -7.357049826291000905, -434.9394999171997824 ) ) ;
#870 = PRODUCT_DEFINITION_CONTEXT ( 'detailed design', #5238, 'design' ) ;
#871 = DIRECTION ( 'NONE',  ( 0.000000000000000000, 0.000000000000000000, -1.000000000000000000 ) ) ;
#872 = CARTESIAN_POINT ( 'NONE',  ( 14.00145308865741711, -5.362717611231083481, -315.0000000000000000 ) ) ;
#873 = ORIENTED_EDGE ( 'NONE', *, *, #6547, .F. ) ;
#874 = CARTESIAN_POINT ( 'NONE',  ( -8.037373804805000077, 9.179324345868998591, -314.4963898845653603 ) ) ;
#875 = ORIENTED_EDGE ( 'NONE', *, *, #1881, .F. ) ;
#876 = CARTESIAN_POINT ( 'NONE',  ( 18.99987372849000167, 0.5562009942294000586, -317.4999999998989892 ) ) ;
#877 = EDGE_LOOP ( 'NONE', ( #3684, #7845, #2714, #438 ) ) ;
#878 = AXIS2_PLACEMENT_3D ( 'NONE', #2871, #7754, #8553 ) ;
#879 = CARTESIAN_POINT ( 'NONE',  ( -20.01660392705000646, -0.3690847706228002623, -303.6197174156509391 ) ) ;
#880 = EDGE_CURVE ( 'NONE', #5498, #146, #2568, .T. ) ;
#881 = DIRECTION ( 'NONE',  ( 1.235123114895485641E-12, 1.000000000000000000, 4.329869796038106469E-12 ) ) ;
#882 = DIRECTION ( 'NONE',  ( 0.000000000000000000, -1.000000000000000000, 0.000000000000000000 ) ) ;
#883 = FILL_AREA_STYLE ('',( #2348 ) ) ;
#884 = CARTESIAN_POINT ( 'NONE',  ( 5.254364691879999327, 12.06635523715000424, -303.6197174156520759 ) ) ;
#885 = LINE ( 'NONE', #2614, #8061 ) ;
#886 = VERTEX_POINT ( 'NONE', #9177 ) ;
#887 = CARTESIAN_POINT ( 'NONE',  ( -2.000000000000000000, -9.500000000000000000, -409.5000000000000000 ) ) ;
#888 = ADVANCED_FACE ( 'NONE', ( #8362 ), #4180, .T. ) ;
#889 = DIRECTION ( 'NONE',  ( 0.000000000000000000, -1.000000000000000000, 0.000000000000000000 ) ) ;
#890 = VERTEX_POINT ( 'NONE', #6702 ) ;
#891 = AXIS2_PLACEMENT_3D ( 'NONE', #2634, #7571, #8267 ) ;
#892 = CARTESIAN_POINT ( 'NONE',  ( 6.420662313211997763, -11.93024803506000531, 190.4207385301700128 ) ) ;
#893 = DIRECTION ( 'NONE',  ( 0.000000000000000000, 1.000000000000000000, 0.000000000000000000 ) ) ;
#894 = CARTESIAN_POINT ( 'NONE',  ( 15.06645494800450891, 4.378519400638148262, -315.0000000000000568 ) ) ;
#895 = CYLINDRICAL_SURFACE ( 'NONE', #7546, 13.99999999999999645 ) ;
#896 = CARTESIAN_POINT ( 'NONE',  ( -11.20196042648000123, 10.44833032063000111, 190.4207385301700128 ) ) ;
#897 = CARTESIAN_POINT ( 'NONE',  ( 13.24479143485999977, -5.858166912337999577, 315.0848619657999734 ) ) ;
#898 = FILL_AREA_STYLE_COLOUR ( '', #2976 ) ;
#899 = EDGE_CURVE ( 'NONE', #830, #7069, #5948, .T. ) ;
#900 = LINE ( 'NONE', #1923, #3134 ) ;
#901 = CARTESIAN_POINT ( 'NONE',  ( 19.57081977481000834, 0.3814303831828999014, 320.0770942683900557 ) ) ;
#902 = DIRECTION ( 'NONE',  ( -0.4712473909295827323, 0.000000000000000000, 0.8820010751365675583 ) ) ;
#903 =( NAMED_UNIT ( * ) SI_UNIT ( $, .STERADIAN. ) SOLID_ANGLE_UNIT ( ) );
#904 = CARTESIAN_POINT ( 'NONE',  ( 6.273744347102000241, 8.772995918477999311, 315.0848619657999734 ) ) ;
#905 = ORIENTED_EDGE ( 'NONE', *, *, #10218, .F. ) ;
#906 = CARTESIAN_POINT ( 'NONE',  ( -28.01838671672000203, 2.500000000000000000, -497.7560445212000104 ) ) ;
#907 = ORIENTED_EDGE ( 'NONE', *, *, #4640, .T. ) ;
#908 = CARTESIAN_POINT ( 'NONE',  ( -5.874649674696526880, -3.342435975618997634, -436.3259412683626692 ) ) ;
#909 = CARTESIAN_POINT ( 'NONE',  ( -11.54746845216141082, 6.952771041492575854, 315.0000000000000000 ) ) ;
#910 = DIRECTION ( 'NONE',  ( 0.000000000000000000, 1.000000000000000000, 0.000000000000000000 ) ) ;
#911 = VERTEX_POINT ( 'NONE', #2564 ) ;
#912 = LINE ( 'NONE', #4202, #6782 ) ;
#913 = ADVANCED_FACE ( 'NONE', ( #1817 ), #9980, .T. ) ;
#914 = MECHANICAL_DESIGN_GEOMETRIC_PRESENTATION_REPRESENTATION (  '', ( #6938 ), #7105 ) ;
#915 = CARTESIAN_POINT ( 'NONE',  ( 14.18540515794000001, 7.627402598852000004, 190.0000000000000000 ) ) ;
#916 = DIRECTION ( 'NONE',  ( 0.000000000000000000, 1.000000000000000000, -0.000000000000000000 ) ) ;
#917 = CARTESIAN_POINT ( 'NONE',  ( 0.000000000000000000, 7.937240849781000307, -284.9999999999999432 ) ) ;
#918 = CARTESIAN_POINT ( 'NONE',  ( -72.90663470102438737, -2.500000000000000444, -371.7168990826883714 ) ) ;
#919 = CARTESIAN_POINT ( 'NONE',  ( 7.863726017345004315, 11.49810175465000661, -316.3802825947000201 ) ) ;
#920 = CARTESIAN_POINT ( 'NONE',  ( -72.90663470102438737, -12.50000000000000000, -371.7168990826883714 ) ) ;
#921 = AXIS2_PLACEMENT_3D ( 'NONE', #9148, #6732, #8389 ) ;
#922 = CARTESIAN_POINT ( 'NONE',  ( -0.9319947458880994962, -7.428963293140000701, -434.5389931698585428 ) ) ;
#923 = DIRECTION ( 'NONE',  ( 0.000000000000000000, 0.000000000000000000, 1.000000000000000000 ) ) ;
#924 = AXIS2_PLACEMENT_3D ( 'NONE', #8563, #5191, #9486 ) ;
#925 = CARTESIAN_POINT ( 'NONE',  ( 13.64075175739776924, -5.653800323622448332, -315.0000000000000000 ) ) ;
#926 = VECTOR ( 'NONE', #7594, 1000.000000000000227 ) ;
#927 = ORIENTED_EDGE ( 'NONE', *, *, #1491, .T. ) ;
#928 = CARTESIAN_POINT ( 'NONE',  ( 0.000000000000000000, 10.54711710274999881, -314.4963898845653603 ) ) ;
#929 = AXIS2_PLACEMENT_3D ( 'NONE', #6785, #1073, #8433 ) ;
#930 = ORIENTED_EDGE ( 'NONE', *, *, #1348, .T. ) ;
#931 = DIRECTION ( 'NONE',  ( -1.000000000000000000, 0.000000000000000000, 0.000000000000000000 ) ) ;
#932 = VERTEX_POINT ( 'NONE', #9124 ) ;
#933 = CIRCLE ( 'NONE', #9689, 10.00000000000000178 ) ;
#934 = CARTESIAN_POINT ( 'NONE',  ( 6.550050338814993545, -11.90210887660999184, -302.9207377450070453 ) ) ;
#935 = CARTESIAN_POINT ( 'NONE',  ( -3.239095488904002007, -11.22417384501999038, -317.4928077629770087 ) ) ;
#936 = FACE_OUTER_BOUND ( 'NONE', #3393, .T. ) ;
#937 = PRODUCT_RELATED_PRODUCT_CATEGORY ( 'part', '', ( #4677 ) ) ;
#938 = VECTOR ( 'NONE', #1431, 1000.000000000000000 ) ;
#939 = SURFACE_SIDE_STYLE ('',( #3206 ) ) ;
#940 = AXIS2_PLACEMENT_3D ( 'NONE', #6757, #144, #6590 ) ;
#941 = CARTESIAN_POINT ( 'NONE',  ( 11.70175841024000185, 10.14170047206000014, -303.6197174156520759 ) ) ;
#942 = CARTESIAN_POINT ( 'NONE',  ( -13.64771691246352781, -6.290639962997291335, 314.4999474536514299 ) ) ;
#943 = ORIENTED_EDGE ( 'NONE', *, *, #3912, .F. ) ;
#944 = PLANE ( 'NONE',  #427 ) ;
#945 = CARTESIAN_POINT ( 'NONE',  ( -2.000000000003786749, -9.500000000000001776, -409.4999999999758415 ) ) ;
#946 = ORIENTED_EDGE ( 'NONE', *, *, #9826, .T. ) ;
#947 = CARTESIAN_POINT ( 'NONE',  ( 19.77421425755001039, -1.922351829117000976, 191.1197171614399792 ) ) ;
#948 = DIRECTION ( 'NONE',  ( 0.000000000000000000, -1.000000000000000000, 0.000000000000000000 ) ) ;
#949 = CARTESIAN_POINT ( 'NONE',  ( 11.65180110541762737, 6.897852064324585974, -315.0000000000000000 ) ) ;
#950 = FACE_OUTER_BOUND ( 'NONE', #7230, .T. ) ;
#951 = CARTESIAN_POINT ( 'NONE',  ( 2.648868200019002472, 12.40196232477001459, 191.1197171614399792 ) ) ;
#952 = CARTESIAN_POINT ( 'NONE',  ( 16.92217352393999974, -0.01966449385450000364, 315.0848619657999734 ) ) ;
#953 = DIRECTION ( 'NONE',  ( -0.4712473909295860630, 0.000000000000000000, 0.8820010751365656709 ) ) ;
#954 = CARTESIAN_POINT ( 'NONE',  ( -7.740399053647997185, -11.10168159160000201, 320.0770942683900557 ) ) ;
#955 = CARTESIAN_POINT ( 'NONE',  ( -9.425149215659013535, 8.435515111409248590, 314.4999430218502425 ) ) ;
#956 = CARTESIAN_POINT ( 'NONE',  ( -14.97723399828063506, 8.302382553459795034, -303.5000000000000000 ) ) ;
#957 = CARTESIAN_POINT ( 'NONE',  ( 17.59334121105999671, 0.04733121045982999903, 314.4150829855000211 ) ) ;
#958 = EDGE_LOOP ( 'NONE', ( #5843, #3891, #8722, #3360 ) ) ;
#959 = CARTESIAN_POINT ( 'NONE',  ( 3.129133257132350465, -12.36387889853562960, 190.9999999999995737 ) ) ;
#960 = CARTESIAN_POINT ( 'NONE',  ( -20.04253597850999569, 0.9484392003694999129, 319.5792614743400009 ) ) ;
#961 = ORIENTED_EDGE ( 'NONE', *, *, #4838, .F. ) ;
#962 = AXIS2_PLACEMENT_3D ( 'NONE', #6233, #2859, #7795 ) ;
#963 = EDGE_CURVE ( 'NONE', #6682, #9889, #2741, .T. ) ;
#964 = ADVANCED_FACE ( 'NONE', ( #9287 ), #358, .F. ) ;
#965 = CARTESIAN_POINT ( 'NONE',  ( -11.73517431002995970, -4.202811174509099246, -438.1641048472901616 ) ) ;
#966 = ADVANCED_BREP_SHAPE_REPRESENTATION ( '', ( #5138, #2817 ), #4734 ) ;
#967 = CARTESIAN_POINT ( 'NONE',  ( -11.72570362167166635, 6.858483604278664103, 315.0000000000000000 ) ) ;
#968 = DIRECTION ( 'NONE',  ( 0.000000000000000000, 1.000000000000000000, -0.000000000000000000 ) ) ;
#969 = ORIENTED_EDGE ( 'NONE', *, *, #8738, .F. ) ;
#970 = CARTESIAN_POINT ( 'NONE',  ( -0.1867348994714999877, -11.51775814840000045, -302.5000000000000000 ) ) ;
#971 =( LENGTH_UNIT ( ) NAMED_UNIT ( * ) SI_UNIT ( .MILLI., .METRE. ) );
#972 = CARTESIAN_POINT ( 'NONE',  ( -4.039076881902885496, -6.821318530964001425, -435.8791522177131696 ) ) ;
#973 = CARTESIAN_POINT ( 'NONE',  ( -15.48916725177958220, 3.890278845006961195, -314.9999999999999432 ) ) ;
#974 = CARTESIAN_POINT ( 'NONE',  ( -46.74071243416547361, -2.500000000000000000, -414.3237589990478114 ) ) ;
#975 = DIRECTION ( 'NONE',  ( -0.2951854283188053429, 0.000000000000000000, 0.9554399839384174475 ) ) ;
#976 = CARTESIAN_POINT ( 'NONE',  ( 19.95007997204999839, 1.762487863542002486, -317.0792622552969533 ) ) ;
#977 = EDGE_CURVE ( 'NONE', #5188, #932, #681, .T. ) ;
#978 = CARTESIAN_POINT ( 'NONE',  ( 14.00000000000000000, -2.500000000000000000, -410.4979246179000256 ) ) ;
#979 = CARTESIAN_POINT ( 'NONE',  ( 8.820893615063965854, -5.815056166419472206, -525.5682599993908752 ) ) ;
#980 = CARTESIAN_POINT ( 'NONE',  ( 14.00000000000000000, -2.500000000000000000, -317.5000000000000000 ) ) ;
#981 = CARTESIAN_POINT ( 'NONE',  ( -0.3940538687071432067, -9.499927474253880177, -315.0000000000000568 ) ) ;
#982 = VERTEX_POINT ( 'NONE', #8517 ) ;
#983 = CARTESIAN_POINT ( 'NONE',  ( 17.50000000000125766, -0.2304358844820579011, -314.4997350343306266 ) ) ;
#984 = CARTESIAN_POINT ( 'NONE',  ( 9.374494192145222726, -11.05367988180385197, -316.5000000000004547 ) ) ;
#985 = ORIENTED_EDGE ( 'NONE', *, *, #6547, .T. ) ;
#986 = CARTESIAN_POINT ( 'NONE',  ( 15.26883884775999967, 6.827716174106000402, -317.5000000000000000 ) ) ;
#987 = ORIENTED_EDGE ( 'NONE', *, *, #4625, .F. ) ;
#988 = CARTESIAN_POINT ( 'NONE',  ( 7.947966332010000023, -11.56278913298000077, -302.9207377450070453 ) ) ;
#989 = CARTESIAN_POINT ( 'NONE',  ( 9.242264416715993747, -10.65406548831999878, -317.5770954168139610 ) ) ;
#990 = CARTESIAN_POINT ( 'NONE',  ( -15.74033075358999945, 3.452242816619000010, -315.0848619657999734 ) ) ;
#991 = PRESENTATION_STYLE_ASSIGNMENT (( #2911 ) ) ;
#992 = CARTESIAN_POINT ( 'NONE',  ( 1.983590419337998734, 12.44807596301999908, -303.6197174156509391 ) ) ;
#993 = DIRECTION ( 'NONE',  ( 0.000000000000000000, -1.000000000000000000, 0.000000000000000000 ) ) ;
#994 = ORIENTED_EDGE ( 'NONE', *, *, #3774, .T. ) ;
#995 = FACE_OUTER_BOUND ( 'NONE', #6467, .T. ) ;
#996 = CARTESIAN_POINT ( 'NONE',  ( -13.37992741786000117, 8.147955808703001068, -302.5000000000000000 ) ) ;
#997 = EDGE_LOOP ( 'NONE', ( #6427, #6798, #10128, #4940 ) ) ;
#998 = CARTESIAN_POINT ( 'NONE',  ( -4.478082317681002955, -12.27758592791000147, 190.4207385301700128 ) ) ;
#999 = DIRECTION ( 'NONE',  ( 0.000000000000000000, -1.000000000000000000, 0.000000000000000000 ) ) ;
#1000 = DIRECTION ( 'NONE',  ( 0.000000000000000000, -1.000000000000000000, 0.000000000000000000 ) ) ;
#1001 = CARTESIAN_POINT ( 'NONE',  ( -1.252197968602001943, 12.57265714642999477, 190.4207385301700128 ) ) ;
#1002 = B_SPLINE_CURVE_WITH_KNOTS ( 'NONE', 3,
 ( #4633, #7160, #7904, #10431, #2110, #3071, #6345, #4521, #7110, #6511, #9846, #5753, #8178, #7372, #9039, #4045, #8278, #2536, #4949, #4849, #2484 ),
 .UNSPECIFIED., .F., .F.,
 ( 4, 1, 1, 1, 2, 2, 2, 2, 1, 1, 2, 2, 4 ),
 ( 0.000000000000000000, 0.1249999999994945710, 0.1874999999991950606, 0.2187499999990910604, 0.2343749999990832888, 0.2499999999990755173, 0.3749999999992109090, 0.4999999999993463007, 0.6249999999994816369, 0.6874999999995808908, 0.7187499999996315170, 0.7499999999996821431, 1.000000000000000000 ),
 .UNSPECIFIED. ) ;
#1003 = EDGE_CURVE ( 'NONE', #7519, #5811, #5243, .T. ) ;
#1004 = CARTESIAN_POINT ( 'NONE',  ( 17.57673583306999632, 0.3313182897943000582, 314.4150829855000211 ) ) ;
#1005 = CARTESIAN_POINT ( 'NONE',  ( -16.11962419174959393, -2.500000000000000000, -430.9361393731155658 ) ) ;
#1006 = CARTESIAN_POINT ( 'NONE',  ( -19.56990143371999125, 0.3944980022354002136, 320.0770942683900557 ) ) ;
#1007 = CARTESIAN_POINT ( 'NONE',  ( -11.05300986228076354, 7.762248751444681183, 314.4999426419797715 ) ) ;
#1008 = CARTESIAN_POINT ( 'NONE',  ( 18.54125634398932121, 4.746072667744948959, -303.4999999999990905 ) ) ;
#1009 = CARTESIAN_POINT ( 'NONE',  ( 15.39920013370999996, 4.579805981517999669, 314.6383426456000052 ) ) ;
#1010 = VERTEX_POINT ( 'NONE', #2776 ) ;
#1011 = DIRECTION ( 'NONE',  ( 0.8820010751365716661, 0.000000000000000000, 0.4712473909295749053 ) ) ;
#1012 = CARTESIAN_POINT ( 'NONE',  ( -20.06808111288002294, -0.4071096865243000185, 319.5792614743400009 ) ) ;
#1013 = ADVANCED_FACE ( 'NONE', ( #6200 ), #2833, .T. ) ;
#1014 = CARTESIAN_POINT ( 'NONE',  ( -4.040158012961684086, -3.178778163799998779, -435.8794274319448050 ) ) ;
#1015 = CARTESIAN_POINT ( 'NONE',  ( -4.578954556310520729, 9.145511589803685837, 315.0000000000000000 ) ) ;
#1016 = CONTEXT_DEPENDENT_SHAPE_REPRESENTATION ( #5098, #7928 ) ;
#1017 = DIRECTION ( 'NONE',  ( 0.000000000000000000, 1.000000000000000000, 0.000000000000000000 ) ) ;
#1018 = ORIENTED_EDGE ( 'NONE', *, *, #5034, .F. ) ;
#1019 = VECTOR ( 'NONE', #2386, 1000.000000000000000 ) ;
#1020 = LINE ( 'NONE', #9142, #9353 ) ;
#1021 = AXIS2_PLACEMENT_3D ( 'NONE', #3288, #1629, #4903 ) ;
#1022 = SURFACE_SIDE_STYLE ('',( #6726 ) ) ;
#1023 = CARTESIAN_POINT ( 'NONE',  ( -10.21689005072306422, -7.047891920729001392, -437.2157279943754133 ) ) ;
#1024 = EDGE_CURVE ( 'NONE', #5654, #10404, #308, .T. ) ;
#1025 = CARTESIAN_POINT ( 'NONE',  ( 16.56500304494299058, -3.264221034209901617, 314.4999403627581387 ) ) ;
#1026 = CARTESIAN_POINT ( 'NONE',  ( -9.285088343672491362, -8.000000000000000000, -419.6576319988688510 ) ) ;
#1027 = DIRECTION ( 'NONE',  ( 0.1736481776669025201, 0.000000000000000000, -0.9848077530122130163 ) ) ;
#1028 = CARTESIAN_POINT ( 'NONE',  ( -41.35482467236749926, -8.000000000000000000, -366.8119992166443808 ) ) ;
#1029 = CARTESIAN_POINT ( 'NONE',  ( 8.337581009124432896, -4.251569741560065729, -525.7130236167810153 ) ) ;
#1030 = CARTESIAN_POINT ( 'NONE',  ( -1.327990674002025528, -7.383908396211002589, -435.1679363805569665 ) ) ;
#1031 = DIRECTION ( 'NONE',  ( -1.000000000000000000, 0.000000000000000000, 0.000000000000000000 ) ) ;
#1032 = CARTESIAN_POINT ( 'NONE',  ( 7.042363285622346147, -8.656086706473070436, -314.9999999999999432 ) ) ;
#1033 = VERTEX_POINT ( 'NONE', #10135 ) ;
#1034 = CARTESIAN_POINT ( 'NONE',  ( -72.90663470096859555, -7.500000000000000000, -371.7168990827444190 ) ) ;
#1035 = AXIS2_PLACEMENT_3D ( 'NONE', #974, #1730, #862 ) ;
#1036 = CARTESIAN_POINT ( 'NONE',  ( -12.80773887004084877, -9.614708322195335555, -316.5000000000004547 ) ) ;
#1037 = ORIENTED_EDGE ( 'NONE', *, *, #4625, .T. ) ;
#1038 = CARTESIAN_POINT ( 'NONE',  ( -46.74071243419621169, -7.500000000000000888, -414.3237589990241077 ) ) ;
#1039 = ORIENTED_EDGE ( 'NONE', *, *, #6534, .T. ) ;
#1040 = AXIS2_PLACEMENT_3D ( 'NONE', #7215, #5321, #6238 ) ;
#1041 = CARTESIAN_POINT ( 'NONE',  ( -19.99999721801999897, -7.771324026006999692E-11, 191.0000000000000000 ) ) ;
#1042 = CARTESIAN_POINT ( 'NONE',  ( 16.58827648083000028, -6.426222433883002516, -317.5770954168139610 ) ) ;
#1043 = CARTESIAN_POINT ( 'NONE',  ( -17.13090252310000139, -0.3058267005333000221, -314.8616023057000461 ) ) ;
#1044 = DIRECTION ( 'NONE',  ( 0.000000000000000000, 0.000000000000000000, 1.000000000000000000 ) ) ;
#1045 =( BOUNDED_CURVE ( )  B_SPLINE_CURVE ( 3, ( #9621, #4574, #8700, #6128 ),
 .UNSPECIFIED., .F., .F. ) 
 B_SPLINE_CURVE_WITH_KNOTS ( ( 4, 4 ),
 ( 0.000000000000000000, 1.000000000000000000 ),
 .UNSPECIFIED. ) 
 CURVE ( )  GEOMETRIC_REPRESENTATION_ITEM ( )  RATIONAL_B_SPLINE_CURVE ( ( 1.017160811567055401, 0.9969340269212683125, 0.9945876386442641381, 1.010121646736042766 ) ) 
 REPRESENTATION_ITEM ( '' )  );
#1046 = CARTESIAN_POINT ( 'NONE',  ( -19.87644374459000929, 1.701742232560001788, -303.6197174156509391 ) ) ;
#1047 = DIRECTION ( 'NONE',  ( -0.9848077530122131273, 0.000000000000000000, -0.1736481776669018817 ) ) ;
#1048 = ORIENTED_EDGE ( 'NONE', *, *, #5342, .F. ) ;
#1049 = CARTESIAN_POINT ( 'NONE',  ( 10.00000000000000000, -2.500000000000000000, -272.5000000000000000 ) ) ;
#1050 = CARTESIAN_POINT ( 'NONE',  ( 9.006891093149000938, 10.12158591819999920, -302.5000000000000000 ) ) ;
#1051 = APPLICATION_CONTEXT ( 'automotive_design' ) ;
#1052 = VERTEX_POINT ( 'NONE', #6047 ) ;
#1053 = CARTESIAN_POINT ( 'NONE',  ( 9.036610176479998202, -11.24204914511999398, 190.4207385301700128 ) ) ;
#1054 = CARTESIAN_POINT ( 'NONE',  ( -10.00000000000000000, -2.500000000000000000, -317.5000000000000000 ) ) ;
#1055 = CARTESIAN_POINT ( 'NONE',  ( -6.445894847559003438, -10.69844988487999693, -302.5071922382879279 ) ) ;
#1056 = CARTESIAN_POINT ( 'NONE',  ( -17.61637523988000353, 5.923742513492005202, 191.1197171614399792 ) ) ;
#1057 = CARTESIAN_POINT ( 'NONE',  ( 4.061138133959000029, -9.851562218542998295, 314.4150829855000211 ) ) ;
#1058 = DIRECTION ( 'NONE',  ( 0.6276613564377035992, 0.000000000000000000, -0.7784864941890654588 ) ) ;
#1059 = CARTESIAN_POINT ( 'NONE',  ( 5.958765323235996725, -11.51784730653000643, 320.0770942683900557 ) ) ;
#1060 = AXIS2_PLACEMENT_3D ( 'NONE', #4551, #2843, #6059 ) ;
#1061 = CARTESIAN_POINT ( 'NONE',  ( -41.41721991556968874, -7.500000000000000888, -366.3159076589344636 ) ) ;
#1062 = CARTESIAN_POINT ( 'NONE',  ( -1.674130924758677530, 12.47364919270561856, -303.5000000000000000 ) ) ;
#1063 = CARTESIAN_POINT ( 'NONE',  ( 3.874983216044999956, 9.425407904674999671, 314.8616023057000461 ) ) ;
#1064 = ORIENTED_EDGE ( 'NONE', *, *, #5099, .F. ) ;
#1065 = DIRECTION ( 'NONE',  ( -0.2756373558170050475, 0.000000000000000000, 0.9612616959383172288 ) ) ;
#1066 = CARTESIAN_POINT ( 'NONE',  ( -18.75338617474996994, 4.519296150162002590, 319.5792614743400009 ) ) ;
#1067 = AXIS2_PLACEMENT_3D ( 'NONE', #5715, #8290, #4217 ) ;
#1068 = CIRCLE ( 'NONE', #2792, 12.50000000613000850 ) ;
#1069 = CARTESIAN_POINT ( 'NONE',  ( -1.437615631311345288, -2.692042927306998568, -435.8453383182137486 ) ) ;
#1070 = CARTESIAN_POINT ( 'NONE',  ( -3.970161185191127817, 9.235879793686278205, 315.0000000000000000 ) ) ;
#1071 = DIRECTION ( 'NONE',  ( -0.2951854283187965167, 0.000000000000000000, 0.9554399839384203341 ) ) ;
#1072 = CARTESIAN_POINT ( 'NONE',  ( -0.9894400438770221129, -2.521929977679939316, -434.4064049843834141 ) ) ;
#1073 = DIRECTION ( 'NONE',  ( 0.000000000000000000, 0.000000000000000000, 1.000000000000000000 ) ) ;
#1074 = CARTESIAN_POINT ( 'NONE',  ( -8.039695956235750174, -7.171008361171001155, -436.6144689615417747 ) ) ;
#1075 = CARTESIAN_POINT ( 'NONE',  ( -14.21145943247442922, 5.188748475648758074, -315.0000000000000000 ) ) ;
#1076 = CIRCLE ( 'NONE', #229, 10.00000000000001599 ) ;
#1077 = CARTESIAN_POINT ( 'NONE',  ( -26.31853765676889267, -9.000000000000001776, -432.7407288192795249 ) ) ;
#1078 = DIRECTION ( 'NONE',  ( 0.000000000000000000, -1.000000000000000000, 0.000000000000000000 ) ) ;
#1079 = DIRECTION ( 'NONE',  ( 0.000000000000000000, -1.000000000000000000, 0.000000000000000000 ) ) ;
#1080 = ADVANCED_FACE ( 'NONE', ( #10245 ), #3998, .T. ) ;
#1081 = FACE_OUTER_BOUND ( 'NONE', #780, .T. ) ;
#1082 = UNCERTAINTY_MEASURE_WITH_UNIT (LENGTH_MEASURE( 1.000000000000000082E-05 ), #1763, 'distance_accuracy_value', 'NONE');
#1083 = DIRECTION ( 'NONE',  ( 0.000000000000000000, 1.000000000000000000, 0.000000000000000000 ) ) ;
#1084 = EDGE_CURVE ( 'NONE', #6576, #215, #8309, .T. ) ;
#1085 = VERTEX_POINT ( 'NONE', #1041 ) ;
#1086 = CARTESIAN_POINT ( 'NONE',  ( 11.73041118561999951, 8.897639792529000502, 319.9928079742500131 ) ) ;
#1087 = CARTESIAN_POINT ( 'NONE',  ( -10.46398288055045889, -10.66551579990979626, -316.5000000000004547 ) ) ;
#1088 = ORIENTED_EDGE ( 'NONE', *, *, #313, .F. ) ;
#1089 = CARTESIAN_POINT ( 'NONE',  ( -2.000000000003786749, -9.500000000000001776, -409.4999999999758415 ) ) ;
#1090 = ORIENTED_EDGE ( 'NONE', *, *, #9756, .T. ) ;
#1091 = CARTESIAN_POINT ( 'NONE',  ( -9.542482902900836450, -2.500000000000000000, -498.6999609700373526 ) ) ;
#1092 = CARTESIAN_POINT ( 'NONE',  ( -11.21026319665000948, -9.143022107836994650, -317.4928077629770087 ) ) ;
#1093 = CIRCLE ( 'NONE', #4515, 5.000000000000008882 ) ;
#1094 = ADVANCED_FACE ( 'NONE', ( #9274 ), #5124, .T. ) ;
#1095 = CARTESIAN_POINT ( 'NONE',  ( -15.10708484062000068, 4.236041382665999500, -315.0848619657999734 ) ) ;
#1096 = EDGE_CURVE ( 'NONE', #4161, #1542, #7598, .T. ) ;
#1097 = CARTESIAN_POINT ( 'NONE',  ( 13.84663869404834102, 6.024484023773909236, -314.5809261257323897 ) ) ;
#1098 = CIRCLE ( 'NONE', #1446, 4.000000000000000000 ) ;
#1099 = CARTESIAN_POINT ( 'NONE',  ( -3.214697847761800006E-15, 10.00000000000000000, 314.4999507458385892 ) ) ;
#1100 = ORIENTED_EDGE ( 'NONE', *, *, #6861, .T. ) ;
#1101 = CARTESIAN_POINT ( 'NONE',  ( -18.53584076651999979, -2.541936159385000060, 190.0000000000000000 ) ) ;
#1102 = FACE_OUTER_BOUND ( 'NONE', #1741, .T. ) ;
#1103 = ORIENTED_EDGE ( 'NONE', *, *, #7129, .T. ) ;
#1104 = CARTESIAN_POINT ( 'NONE',  ( -19.96348645057001647, -0.8966426439394996617, 191.1197171614399792 ) ) ;
#1105 = VERTEX_POINT ( 'NONE', #6138 ) ;
#1106 = CARTESIAN_POINT ( 'NONE',  ( -82.18980308971114823, -2.500000000000000000, -388.2946789300659134 ) ) ;
#1107 = CARTESIAN_POINT ( 'NONE',  ( 18.90089112233000179, -0.2930644900430999789, -302.5071922382879279 ) ) ;
#1108 = CARTESIAN_POINT ( 'NONE',  ( -19.12235363464000670, 3.679291565416002108, 191.1197171614399792 ) ) ;
#1109 = APPLICATION_CONTEXT ( 'automotive_design' ) ;
#1110 = CIRCLE ( 'NONE', #2316, 0.7499999999999997780 ) ;
#1111 = AXIS2_PLACEMENT_3D ( 'NONE', #8004, #8802, #4672 ) ;
#1112 = AXIS2_PLACEMENT_3D ( 'NONE', #4461, #4312, #279 ) ;
#1113 = EDGE_CURVE ( 'NONE', #2720, #1085, #9682, .T. ) ;
#1114 = CARTESIAN_POINT ( 'NONE',  ( -0.9643324756131976816, -7.495094651894998350, -434.3305354681787662 ) ) ;
#1115 = FACE_OUTER_BOUND ( 'NONE', #8891, .T. ) ;
#1116 = CARTESIAN_POINT ( 'NONE',  ( 20.08948270067001829, -0.1023867585008999687, 319.5792614743400009 ) ) ;
#1117 = CARTESIAN_POINT ( 'NONE',  ( -17.50000000000000711, 8.653878165429867666E-10, 190.0000000000001137 ) ) ;
#1118 = CARTESIAN_POINT ( 'NONE',  ( 1.276003512426000075, 9.874146089817999794, 314.6383426456000052 ) ) ;
#1119 = ORIENTED_EDGE ( 'NONE', *, *, #7066, .F. ) ;
#1120 = CARTESIAN_POINT ( 'NONE',  ( 16.77317840633001467, -5.196478383294000025, 190.0071920248299477 ) ) ;
#1121 = ORIENTED_EDGE ( 'NONE', *, *, #9520, .F. ) ;
#1122 = CARTESIAN_POINT ( 'NONE',  ( 13.19336277821000536, 9.492603533888004819, 319.5792614743400009 ) ) ;
#1123 = LINE ( 'NONE', #1174, #4934 ) ;
#1124 = CARTESIAN_POINT ( 'NONE',  ( 5.241997271368903810, 9.033710068163633977, 315.0000000000000000 ) ) ;
#1125 = ADVANCED_FACE ( 'NONE', ( #9324 ), #8817, .T. ) ;
#1126 = LINE ( 'NONE', #2795, #10298 ) ;
#1127 = STYLED_ITEM ( 'NONE', ( #1697 ), #7250 ) ;
#1128 = CARTESIAN_POINT ( 'NONE',  ( -72.90663470096859555, -7.500000000000000000, -371.7168990827444190 ) ) ;
#1129 = PRESENTATION_STYLE_ASSIGNMENT (( #3395 ) ) ;
#1130 = CARTESIAN_POINT ( 'NONE',  ( -3.134365345935000047, 11.35765845234000082, 190.0000000000000000 ) ) ;
#1131 =( BOUNDED_SURFACE ( )  B_SPLINE_SURFACE ( 3, 3, ( 
 ( #4380, #2815, #5228, #2715, #3724, #246, #2867, #9377, #5981, #7010, #3522, #6801, #2011, #5178, #4425, #7651, #3570, #6852, #10121, #6032, #8505, #2663, #7701, #3624, #5276, #1193, #4472, #10233, #5324, #8600, #1248, #4524, #7804, #5930, #9221, #1854, #9581, #2918, #10486, #8878, #2220 ),
 ( #7858, #613, #1520, #6406, #1302, #503, #2113, #6186, #7114, #5379, #4800, #7163, #5596, #8072, #4636, #2970, #3074, #10434, #10281, #6241, #8660, #4582, #7064, #5433, #7218, #10329, #3128, #8767, #9527, #1408, #2167, #8711, #3886, #8822, #6348, #716, #3989, #9472, #1354, #9686, #2328 ),
 ( #9630, #7907, #552, #3829, #10382, #2272, #3771, #5488, #3022, #5538, #6296, #4691, #7967, #1468, #4749, #8019, #662, #3938, #4097, #7483, #8181, #125, #4902, #7375, #3238, #4853, #9149, #864, #2540, #2595, #817, #11, #3287, #6568, #10596, #9849, #6514, #976, #2487, #8338, #5756 ),
 ( #4152, #1575, #7430, #6626, #9954, #9044, #1679, #68, #3347, #4952, #8228, #9904, #8990, #5857, #3402, #5806, #9796, #9097, #1732, #5001, #1628, #1787, #4209, #8282, #6675, #919, #5057, #8128, #7271, #10542, #5646, #7325, #3186, #6459, #9740, #8931, #2382, #765, #4048, #2434, #5704 ) ),
 .UNSPECIFIED., .F., .F., .F. ) 
 B_SPLINE_SURFACE_WITH_KNOTS ( ( 4, 4 ),
 ( 4, 1, 1, 1, 1, 1, 1, 1, 1, 1, 1, 1, 1, 1, 1, 1, 1, 1, 1, 1, 1, 1, 1, 1, 1, 1, 1, 1, 1, 1, 1, 1, 1, 1, 1, 1, 1, 1, 4 ),
 ( 0.000000000000000000, 1.000000000000000000 ),
 ( -0.007738640450444999631, 0.000000000000000000, 0.03414709649185000001, 0.06696605908318999101, 0.09596079224771000837, 0.1211002772268999911, 0.1443783404606999998, 0.1680876537897000034, 0.1921286104184000143, 0.2160216200219000071, 0.2397245863996999848, 0.2634813019505999887, 0.2879188160025000220, 0.3133917475886000004, 0.3395543376315999784, 0.3663618195672999622, 0.3946229251345000355, 0.4252536485549999745, 0.4591139563344999730, 0.4956048897295999844, 0.5324779435423999674, 0.5674158629142000976, 0.5992726300609999557, 0.6287198090143000240, 0.6565915576515000129, 0.6836661054489000522, 0.7100337132233999204, 0.7353920520230999847, 0.7598724402797999433, 0.7838392479475999597, 0.8076909583479000565, 0.8317349054331000247, 0.8555088018188000687, 0.8788217029082999732, 0.9039691640437000908, 0.9329692239710999369, 0.9658153655582000230, 1.000000000000000000, 1.008464120473999914 ),
 .UNSPECIFIED. ) 
 GEOMETRIC_REPRESENTATION_ITEM ( )  RATIONAL_B_SPLINE_SURFACE ( (
 ( 1.236577356246000070, 1.236577356246000070, 1.236577356246000070, 1.236577356246000070, 1.236577356246000070, 1.236577356246000070, 1.236577356246000070, 1.236577356246000070, 1.236577356246000070, 1.236577356246000070, 1.236577356246000070, 1.236577356246000070, 1.236577356246000070, 1.236577356246000070, 1.236577356246000070, 1.236577356246000070, 1.236577356246000070, 1.236577356246000070, 1.236577356246000070, 1.236577356246000070, 1.236577356246000070, 1.236577356246000070, 1.236577356246000070, 1.236577356246000070, 1.236577356246000070, 1.236577356246000070, 1.236577356246000070, 1.236577356246000070, 1.236577356246000070, 1.236577356246000070, 1.236577356246000070, 1.236577356246000070, 1.236577356246000070, 1.236577356246000070, 1.236577356246000070, 1.236577356246000070, 1.236577356246000070, 1.236577356246000070, 1.236577356246000070, 1.236577356246000070, 1.236577356246000070),
 ( 0.9211408812511999722, 0.9211408812511999722, 0.9211408812511999722, 0.9211408812511999722, 0.9211408812511999722, 0.9211408812511999722, 0.9211408812511999722, 0.9211408812511999722, 0.9211408812511999722, 0.9211408812511999722, 0.9211408812511999722, 0.9211408812511999722, 0.9211408812511999722, 0.9211408812511999722, 0.9211408812511999722, 0.9211408812511999722, 0.9211408812511999722, 0.9211408812511999722, 0.9211408812511999722, 0.9211408812511999722, 0.9211408812511999722, 0.9211408812511999722, 0.9211408812511999722, 0.9211408812511999722, 0.9211408812511999722, 0.9211408812511999722, 0.9211408812511999722, 0.9211408812511999722, 0.9211408812511999722, 0.9211408812511999722, 0.9211408812511999722, 0.9211408812511999722, 0.9211408812511999722, 0.9211408812511999722, 0.9211408812511999722, 0.9211408812511999722, 0.9211408812511999722, 0.9211408812511999722, 0.9211408812511999722, 0.9211408812511999722, 0.9211408812511999722),
 ( 0.9211408812511999722, 0.9211408812511999722, 0.9211408812511999722, 0.9211408812511999722, 0.9211408812511999722, 0.9211408812511999722, 0.9211408812511999722, 0.9211408812511999722, 0.9211408812511999722, 0.9211408812511999722, 0.9211408812511999722, 0.9211408812511999722, 0.9211408812511999722, 0.9211408812511999722, 0.9211408812511999722, 0.9211408812511999722, 0.9211408812511999722, 0.9211408812511999722, 0.9211408812511999722, 0.9211408812511999722, 0.9211408812511999722, 0.9211408812511999722, 0.9211408812511999722, 0.9211408812511999722, 0.9211408812511999722, 0.9211408812511999722, 0.9211408812511999722, 0.9211408812511999722, 0.9211408812511999722, 0.9211408812511999722, 0.9211408812511999722, 0.9211408812511999722, 0.9211408812511999722, 0.9211408812511999722, 0.9211408812511999722, 0.9211408812511999722, 0.9211408812511999722, 0.9211408812511999722, 0.9211408812511999722, 0.9211408812511999722, 0.9211408812511999722),
 ( 1.236577356246000070, 1.236577356246000070, 1.236577356246000070, 1.236577356246000070, 1.236577356246000070, 1.236577356246000070, 1.236577356246000070, 1.236577356246000070, 1.236577356246000070, 1.236577356246000070, 1.236577356246000070, 1.236577356246000070, 1.236577356246000070, 1.236577356246000070, 1.236577356246000070, 1.236577356246000070, 1.236577356246000070, 1.236577356246000070, 1.236577356246000070, 1.236577356246000070, 1.236577356246000070, 1.236577356246000070, 1.236577356246000070, 1.236577356246000070, 1.236577356246000070, 1.236577356246000070, 1.236577356246000070, 1.236577356246000070, 1.236577356246000070, 1.236577356246000070, 1.236577356246000070, 1.236577356246000070, 1.236577356246000070, 1.236577356246000070, 1.236577356246000070, 1.236577356246000070, 1.236577356246000070, 1.236577356246000070, 1.236577356246000070, 1.236577356246000070, 1.236577356246000070) ) ) 
 REPRESENTATION_ITEM ( '' )  SURFACE ( )  );
#1132 = CARTESIAN_POINT ( 'NONE',  ( 8.203579894969822206, -8.842447374029218210, 314.4999432750969390 ) ) ;
#1133 = CARTESIAN_POINT ( 'NONE',  ( -17.27977314787002427, 4.562413721234999109, 190.0071920248299477 ) ) ;
#1134 = CARTESIAN_POINT ( 'NONE',  ( -27.98005464532998232, -9.000000000000001776, -417.3300389808354680 ) ) ;
#1135 = AXIS2_PLACEMENT_3D ( 'NONE', #9570, #2425, #10533 ) ;
#1136 = DIRECTION ( 'NONE',  ( 0.000000000000000000, -1.000000000000000000, -0.000000000000000000 ) ) ;
#1137 = ADVANCED_FACE ( 'NONE', ( #1145 ), #10198, .T. ) ;
#1138 = DIRECTION ( 'NONE',  ( 0.1247904863035890766, 0.000000000000000000, -0.9921831154218024862 ) ) ;
#1139 = DIRECTION ( 'NONE',  ( -0.9627072696281171460, 0.1321637200910011078, -0.2360666518102109701 ) ) ;
#1140 = ORIENTED_EDGE ( 'NONE', *, *, #4953, .T. ) ;
#1141 = CARTESIAN_POINT ( 'NONE',  ( 18.70127769336001222, 1.615776359209001312, 319.9928079742500131 ) ) ;
#1142 = CARTESIAN_POINT ( 'NONE',  ( 19.86884641856056533, -1.746738893747486809, -316.5000000000004547 ) ) ;
#1143 = CARTESIAN_POINT ( 'NONE',  ( 14.00000000000000000, -2.500000000000000000, -317.5000000000000000 ) ) ;
#1144 = ORIENTED_EDGE ( 'NONE', *, *, #2095, .F. ) ;
#1145 = FACE_OUTER_BOUND ( 'NONE', #2200, .T. ) ;
#1146 = EDGE_CURVE ( 'NONE', #2810, #4863, #5556, .T. ) ;
#1147 = CARTESIAN_POINT ( 'NONE',  ( -10.31351018857999513, -10.27238149472999851, -317.5770954168139610 ) ) ;
#1148 = ADVANCED_FACE ( 'NONE', ( #7751 ), #1131, .T. ) ;
#1149 = PRODUCT_DEFINITION_SHAPE ( 'NONE', 'NONE',  #10632 ) ;
#1150 = DIRECTION ( 'NONE',  ( 0.1247904863035921574, 0.000000000000000000, -0.9921831154218020421 ) ) ;
#1151 = DIRECTION ( 'NONE',  ( 0.000000000000000000, 1.000000000000000000, 0.000000000000000000 ) ) ;
#1152 = ORIENTED_EDGE ( 'NONE', *, *, #4382, .T. ) ;
#1153 = CARTESIAN_POINT ( 'NONE',  ( -19.00000000000000000, 0.000000000000000000, 190.0000000000100044 ) ) ;
#1154 = CARTESIAN_POINT ( 'NONE',  ( -14.88027513490713893, -8.363422937417031022, 319.0000000000003979 ) ) ;
#1155 = EDGE_LOOP ( 'NONE', ( #7696, #1064, #1796, #10507 ) ) ;
#1156 = CARTESIAN_POINT ( 'NONE',  ( -19.32351226214659690, 3.349534253028545461, -316.5000000000004547 ) ) ;
#1157 = ORIENTED_EDGE ( 'NONE', *, *, #2791, .F. ) ;
#1158 = CARTESIAN_POINT ( 'NONE',  ( -16.37744599325981909, -2.527607301898085801, 314.9999999999999432 ) ) ;
#1159 = B_SPLINE_CURVE_WITH_KNOTS ( 'NONE', 3,
 ( #4416, #8440, #10011, #3561, #979, #5920, #182, #6678, #127, #8392, #9369, #2003, #10113, #9958, #5860, #7693, #7587, #1949, #2753, #336, #4211, #3404, #5115, #3613, #1843, #236, #3456, #5060, #5267, #4370, #9315 ),
 .UNSPECIFIED., .F., .F.,
 ( 4, 2, 2, 2, 1, 1, 1, 2, 2, 2, 2, 1, 1, 1, 1, 2, 2, 2, 4 ),
 ( 0.000000000000000000, 0.1250000000002775280, 0.1875000000004162504, 0.2187500000004856116, 0.2343750000005130896, 0.2421875000005322132, 0.2460937500005417611, 0.2480468750005504208, 0.2500000000005591083, 0.3750000000010509371, 0.4375000000012961299, 0.4687500000014282464, 0.4843750000015074053, 0.4921875000015624169, 0.4960937500015898949, 0.4980468750016032176, 0.5000000000016164847, 0.7500000000008082424, 1.000000000000000000 ),
 .UNSPECIFIED. ) ;
#1160 = EDGE_CURVE ( 'NONE', #2578, #830, #10540, .T. ) ;
#1161 = CARTESIAN_POINT ( 'NONE',  ( 16.34352199340000311, 7.209047878930006092, 191.1197171614399792 ) ) ;
#1162 = CIRCLE ( 'NONE', #3220, 11.00000000000000000 ) ;
#1163 = CARTESIAN_POINT ( 'NONE',  ( -0.8117387980152629412, -7.500462190812000607, -434.2418354198644010 ) ) ;
#1164 = SHAPE_REPRESENTATION_RELATIONSHIP ( 'NONE' , 'NONE' ,  #1739, #966 ) ;
#1165 = CARTESIAN_POINT ( 'NONE',  ( 17.60320223513998172, 4.128492944088002048, -302.5071922382879279 ) ) ;
#1166 = CARTESIAN_POINT ( 'NONE',  ( -20.00482943604999164, -0.07455149923640995435, 318.8802828394900644 ) ) ;
#1167 = CIRCLE ( 'NONE', #7689, 5.000000000000006217 ) ;
#1168 = CARTESIAN_POINT ( 'NONE',  ( 1.279515965483999906E-07, 10.00000000755999885, 190.0000000000000000 ) ) ;
#1169 = CARTESIAN_POINT ( 'NONE',  ( -13.50042001888999899, 6.225262767767000049, 314.6383426456000052 ) ) ;
#1170 = ORIENTED_EDGE ( 'NONE', *, *, #2276, .F. ) ;
#1171 = CARTESIAN_POINT ( 'NONE',  ( -38.33299437316763658, -7.500000000000000000, -461.6435047520546391 ) ) ;
#1172 = CARTESIAN_POINT ( 'NONE',  ( -13.88394749849000043, 9.000054837070988967, 318.8802828394900644 ) ) ;
#1173 = B_SPLINE_SURFACE_WITH_KNOTS ( 'NONE', 3, 1, ( 
 ( #3373, #8463 ),
 ( #4126, #7402 ),
 ( #6650, #6595 ),
 ( #1866, #2677 ),
 ( #148, #4232 ),
 ( #7559, #9877 ),
 ( #3422, #5778 ),
 ( #9070, #7506 ),
 ( #2621, #9979 ),
 ( #5883, #9176 ),
 ( #1816, #8414 ),
 ( #5081, #1705 ),
 ( #7611, #4978 ) ),
 .UNSPECIFIED., .F., .F., .F.,
 ( 4, 1, 1, 1, 1, 1, 1, 1, 1, 1, 4 ),
 ( 2, 2 ),
 ( 0.01923076854978371733, 0.09935897435896999530, 0.1794871794871999993, 0.2596153846154000133, 0.3397435897436000274, 0.5000000000000000000, 0.6602564102564000281, 0.7403846153845999867, 0.8205128205128000562, 0.9006410256410000148, 0.9807692307692000844 ),
 ( 0.000000000000000000, 1.000000000000000000 ),
 .UNSPECIFIED. ) ;
#1174 = CARTESIAN_POINT ( 'NONE',  ( -48.08064548948741646, -9.500000000000001776, -401.8957833228595860 ) ) ;
#1175 = LINE ( 'NONE', #8742, #10006 ) ;
#1176 = CARTESIAN_POINT ( 'NONE',  ( -2.000000000000000000, -9.500000000000000000, -414.5000000000000000 ) ) ;
#1177 = FACE_OUTER_BOUND ( 'NONE', #10616, .T. ) ;
#1178 = CARTESIAN_POINT ( 'NONE',  ( -12.82600522015554922, -5.696851206212700802, -438.3416979569461205 ) ) ;
#1179 = CARTESIAN_POINT ( 'NONE',  ( -15.47196055635296474, 3.911380178888624215, -315.0000000000000568 ) ) ;
#1180 = CARTESIAN_POINT ( 'NONE',  ( -18.85089486759000010, 0.8058634873976002755, 190.0071920248299477 ) ) ;
#1181 = FACE_OUTER_BOUND ( 'NONE', #6826, .T. ) ;
#1182 = DIRECTION ( 'NONE',  ( 0.000000000000000000, -1.000000000000000000, 0.000000000000000000 ) ) ;
#1183 = VECTOR ( 'NONE', #6630, 1000.000000000000114 ) ;
#1184 = AXIS2_PLACEMENT_3D ( 'NONE', #97, #5779, #6762 ) ;
#1185 = DIRECTION ( 'NONE',  ( 0.9848077530122130163, 0.000000000000000000, 0.1736481776669023813 ) ) ;
#1186 = CARTESIAN_POINT ( 'NONE',  ( 4.532266548732788003, -9.152838354191798587, 315.0000000000000568 ) ) ;
#1187 = CARTESIAN_POINT ( 'NONE',  ( 6.370857846455999507, 9.209451711050000711, -314.6383426456000052 ) ) ;
#1188 = EDGE_LOOP ( 'NONE', ( #2072, #8240, #8227, #5008 ) ) ;
#1189 = CARTESIAN_POINT ( 'NONE',  ( -11.51418862744999139, 9.000691300089004088, 319.9928079742500131 ) ) ;
#1190 = CARTESIAN_POINT ( 'NONE',  ( -89.32175647514451100, -2.500000000000000000, -345.2379088676337915 ) ) ;
#1191 = DIRECTION ( 'NONE',  ( -0.000000000000000000, 1.000000000000000000, 0.000000000000000000 ) ) ;
#1192 = ORIENTED_EDGE ( 'NONE', *, *, #9891, .F. ) ;
#1193 = CARTESIAN_POINT ( 'NONE',  ( 7.576881921353003868, 10.42269368856000611, -317.4928077629770087 ) ) ;
#1194 = AXIS2_PLACEMENT_3D ( 'NONE', #4119, #993, #6644 ) ;
#1195 = EDGE_CURVE ( 'NONE', #661, #9639, #384, .T. ) ;
#1196 = CARTESIAN_POINT ( 'NONE',  ( -9.218822326027003911, -11.18653774893999220, -317.0792622552969533 ) ) ;
#1197 = LINE ( 'NONE', #8604, #4995 ) ;
#1198 = COLOUR_RGB ( '', 0.08235294, 0.09019608, 0.10196078) ;
#1199 = EDGE_CURVE ( 'NONE', #6555, #5133, #2654, .T. ) ;
#1200 = CARTESIAN_POINT ( 'NONE',  ( -79.31727611502927289, -7.500000000000000000, -351.2304352734219606 ) ) ;
#1201 = ORIENTED_EDGE ( 'NONE', *, *, #1003, .T. ) ;
#1202 = CARTESIAN_POINT ( 'NONE',  ( -14.94331899262999919, -7.078020551493000134, 190.0000000000000000 ) ) ;
#1203 = EDGE_CURVE ( 'NONE', #10408, #6648, #4023, .T. ) ;
#1204 = CARTESIAN_POINT ( 'NONE',  ( -11.22905947253953762, -10.35317575229728781, 319.0000000000003979 ) ) ;
#1205 = VERTEX_POINT ( 'NONE', #3453 ) ;
#1206 = CARTESIAN_POINT ( 'NONE',  ( -18.70579689905999032, -4.435290649195002821, 191.1197171614399792 ) ) ;
#1207 = VERTEX_POINT ( 'NONE', #2751 ) ;
#1208 = CARTESIAN_POINT ( 'NONE',  ( 6.052780067456072999, -4.500000000000000888, -524.2189112390747141 ) ) ;
#1209 = DIRECTION ( 'NONE',  ( 0.000000000000000000, 1.000000000000000000, -0.000000000000000000 ) ) ;
#1210 = CARTESIAN_POINT ( 'NONE',  ( 17.64332610462000872, 5.892819363352002959, 191.1197171614399792 ) ) ;
#1211 = LINE ( 'NONE', #10139, #9926 ) ;
#1212 = FILL_AREA_STYLE_COLOUR ( '', #7652 ) ;
#1213 = CARTESIAN_POINT ( 'NONE',  ( -8.907970405212992659, 10.02857016715000604, -302.5071922382879279 ) ) ;
#1214 = CARTESIAN_POINT ( 'NONE',  ( -14.87617152917998631, -8.357511890987989744, 318.8802828394900644 ) ) ;
#1215 = LINE ( 'NONE', #2785, #8659 ) ;
#1216 = CARTESIAN_POINT ( 'NONE',  ( -6.388932193737000276, 8.746770244069999478, 315.0848619657999734 ) ) ;
#1217 = EDGE_CURVE ( 'NONE', #5133, #1207, #293, .T. ) ;
#1218 = VERTEX_POINT ( 'NONE', #6075 ) ;
#1219 = CARTESIAN_POINT ( 'NONE',  ( 7.497671121046002973, -10.44264915526000514, 190.0071920248299477 ) ) ;
#1220 = EDGE_LOOP ( 'NONE', ( #1727, #6254 ) ) ;
#1221 = DIRECTION ( 'NONE',  ( 0.000000000000000000, 1.000000000000000000, -0.000000000000000000 ) ) ;
#1222 = DIRECTION ( 'NONE',  ( -0.9712267471052611345, 0.000000000000000000, -0.2381566831044912569 ) ) ;
#1223 = EDGE_CURVE ( 'NONE', #8790, #6146, #8438, .T. ) ;
#1224 = CARTESIAN_POINT ( 'NONE',  ( -17.12450099635000100, 0.4005340032738999856, 314.8616023057000461 ) ) ;
#1225 = DIRECTION ( 'NONE',  ( 0.000000000000000000, 1.000000000000000000, -0.000000000000000000 ) ) ;
#1226 = FACE_OUTER_BOUND ( 'NONE', #9202, .T. ) ;
#1227 = CARTESIAN_POINT ( 'NONE',  ( -8.636340573252621056, -8.171206817651018639, -315.0000000000000568 ) ) ;
#1228 = CARTESIAN_POINT ( 'NONE',  ( -4.443194270446590544, -3.070841006776869886, -436.4083858720387639 ) ) ;
#1229 = LINE ( 'NONE', #6992, #2985 ) ;
#1230 = CARTESIAN_POINT ( 'NONE',  ( 20.00000000000000000, 0.000000000000000000, -303.5000000000000000 ) ) ;
#1231 = CARTESIAN_POINT ( 'NONE',  ( -3.689485142014396590, 9.275849510248953322, -315.0000000000000000 ) ) ;
#1232 = PRODUCT ( 'Handle', 'Handle', '', ( #1399 ) ) ;
#1234 = CARTESIAN_POINT ( 'NONE',  ( 17.30501060709000072, 4.528037784100006569, 190.0071920248299477 ) ) ;
#1233 = AXIS2_PLACEMENT_3D ( 'NONE', #8007, #6501, #4787 ) ;
#1235 = CARTESIAN_POINT ( 'NONE',  ( -17.49999999911142723, 5.867334123717705907, 189.9999999999995453 ) ) ;
#1236 = ORIENTED_EDGE ( 'NONE', *, *, #6395, .F. ) ;
#1237 = CARTESIAN_POINT ( 'NONE',  ( -4.878402812341999351, -11.12254092566999830, -317.5000000000000000 ) ) ;
#1238 = LINE ( 'NONE', #9569, #7592 ) ;
#1239 = ADVANCED_FACE ( 'NONE', ( #4414 ), #6790, .T. ) ;
#1240 = DIRECTION ( 'NONE',  ( 0.000000000000000000, 0.000000000000000000, 1.000000000000000000 ) ) ;
#1241 = CARTESIAN_POINT ( 'NONE',  ( 4.462202093987085227, -9.163742891420229242, 315.0000000000000000 ) ) ;
#1242 = CARTESIAN_POINT ( 'NONE',  ( -4.001463906138999604, 9.408458373209999337, -314.8616023057000461 ) ) ;
#1243 = AXIS2_PLACEMENT_3D ( 'NONE', #4932, #8161, #8048 ) ;
#1244 = CARTESIAN_POINT ( 'NONE',  ( -16.99996037728000076, 1.352916227065999958E-09, 314.9999801883000146 ) ) ;
#1245 = DIRECTION ( 'NONE',  ( 0.000000000000000000, 1.000000000000000000, 0.000000000000000000 ) ) ;
#1246 = DIRECTION ( 'NONE',  ( 0.000000000000000000, 0.000000000000000000, -1.000000000000000000 ) ) ;
#1247 = ORIENTED_EDGE ( 'NONE', *, *, #6953, .F. ) ;
#1248 = CARTESIAN_POINT ( 'NONE',  ( 13.31532601970998897, 8.047348965112000485, -317.4928077629770087 ) ) ;
#1249 = CARTESIAN_POINT ( 'NONE',  ( 0.2369326581469002602, -12.59441454048000608, -317.0792622552969533 ) ) ;
#1250 = CARTESIAN_POINT ( 'NONE',  ( -51.41224207513305799, -12.00000000000000000, -371.0859316413308306 ) ) ;
#1251 = CARTESIAN_POINT ( 'NONE',  ( 0.9204674644685802987, 9.999779064329263889, -314.4999424967811024 ) ) ;
#1252 = EDGE_CURVE ( 'NONE', #6040, #2579, #3555, .T. ) ;
#1253 = ORIENTED_EDGE ( 'NONE', *, *, #1527, .F. ) ;
#1254 = CARTESIAN_POINT ( 'NONE',  ( 11.72056399716000108, -9.035224326960999974, 190.0000000000000000 ) ) ;
#1255 = CARTESIAN_POINT ( 'NONE',  ( -17.65399305443192191, -5.890951312620556379, 319.0000000000003979 ) ) ;
#1256 = CIRCLE ( 'NONE', #6764, 3.500000000000003109 ) ;
#1257 = ORIENTED_EDGE ( 'NONE', *, *, #2987, .F. ) ;
#1258 = CARTESIAN_POINT ( 'NONE',  ( 9.011282031845993856, -11.16162715973000097, 191.1197171614399792 ) ) ;
#1259 = VERTEX_POINT ( 'NONE', #9314 ) ;
#1260 = CARTESIAN_POINT ( 'NONE',  ( -13.30825372127758399, -7.500000000000000888, -400.6612558711213410 ) ) ;
#1261 = CARTESIAN_POINT ( 'NONE',  ( 11.26120837094999594, -9.120087085473000954, -302.5071922382879279 ) ) ;
#1262 = CARTESIAN_POINT ( 'NONE',  ( -37.87192209818999800, 2.500000000000000000, -461.0868123482000556 ) ) ;
#1263 = ORIENTED_EDGE ( 'NONE', *, *, #3216, .T. ) ;
#1264 = STYLED_ITEM ( 'NONE', ( #2643 ), #8937 ) ;
#1265 = CARTESIAN_POINT ( 'NONE',  ( -1.624818744522249503, -7.500000000000000888, -412.9798331893018712 ) ) ;
#1266 = AXIS2_PLACEMENT_3D ( 'NONE', #9096, #5703, #2433 ) ;
#1267 = CARTESIAN_POINT ( 'NONE',  ( -18.70581557644998938, -4.435354026251000725, 318.8802828394900644 ) ) ;
#1268 = CARTESIAN_POINT ( 'NONE',  ( 15.43693218238999876, -4.538485726840999490, -314.6383426456000052 ) ) ;
#1269 = VECTOR ( 'NONE', #6090, 1000.000000000000114 ) ;
#1270 = CARTESIAN_POINT ( 'NONE',  ( -12.28828818102000042, 7.249309191407999897, 314.4150829855000211 ) ) ;
#1271 = ORIENTED_EDGE ( 'NONE', *, *, #7423, .F. ) ;
#1272 = CARTESIAN_POINT ( 'NONE',  ( 18.87263095182001749, 0.3456903499861000983, 190.0071920248299477 ) ) ;
#1273 = ORIENTED_EDGE ( 'NONE', *, *, #1410, .F. ) ;
#1274 = CARTESIAN_POINT ( 'NONE',  ( -1.249129537600907502, -7.462014900586536825, -434.5271252024986666 ) ) ;
#1275 = DIRECTION ( 'NONE',  ( 0.000000000000000000, 1.000000000000000000, 0.000000000000000000 ) ) ;
#1276 = AXIS2_PLACEMENT_3D ( 'NONE', #6620, #9898, #9257 ) ;
#1277 = ADVANCED_FACE ( 'NONE', ( #8390, #4462, #9365, #4264, #6943 ), #4313, .F. ) ;
#1278 = DIRECTION ( 'NONE',  ( -0.9554399839384175586, 0.000000000000000000, -0.2951854283188048989 ) ) ;
#1279 = DIRECTION ( 'NONE',  ( 0.000000000000000000, 1.000000000000000000, -0.000000000000000000 ) ) ;
#1280 = CARTESIAN_POINT ( 'NONE',  ( -15.35630118782766651, 4.050343336346089451, 315.0000000000000000 ) ) ;
#1281 = CARTESIAN_POINT ( 'NONE',  ( 11.28781796570999951, -4.951468039558000633, -284.9999999999999432 ) ) ;
#1282 = AXIS2_PLACEMENT_3D ( 'NONE', #5388, #3631, #4388 ) ;
#1283 = MECHANICAL_DESIGN_GEOMETRIC_PRESENTATION_REPRESENTATION (  '', ( #8325 ), #10048 ) ;
#1284 = CARTESIAN_POINT ( 'NONE',  ( -2.257099744627868443, -9.415190953705950605, -315.0000000000000568 ) ) ;
#1285 = CARTESIAN_POINT ( 'NONE',  ( 4.000000000000000000, 2.656480000000000175, -410.4979246179000256 ) ) ;
#1286 = PLANE ( 'NONE',  #4156 ) ;
#1287 = ADVANCED_FACE ( 'NONE', ( #1841, #7740, #3559 ), #8492, .T. ) ;
#1288 = CARTESIAN_POINT ( 'NONE',  ( -11.93419529315104732, 6.745200168737855329, -315.0000000000000568 ) ) ;
#1289 = CARTESIAN_POINT ( 'NONE',  ( -9.985646804708002477, 10.39189181891999780, 189.9229057364800042 ) ) ;
#1290 = CARTESIAN_POINT ( 'NONE',  ( 7.420201433257000545, 2.500000000000000000, -419.8948508258000061 ) ) ;
#1291 = ADVANCED_FACE ( 'NONE', ( #1181 ), #10221, .T. ) ;
#1292 = ORIENTED_EDGE ( 'NONE', *, *, #10149, .T. ) ;
#1293 = CARTESIAN_POINT ( 'NONE',  ( -15.26883884775999967, -6.827716174106000402, -317.5000000000000000 ) ) ;
#1294 = CARTESIAN_POINT ( 'NONE',  ( -50.43337757792475173, -7.500000000000000000, -464.9351226150769207 ) ) ;
#1295 = CARTESIAN_POINT ( 'NONE',  ( 16.61594764501906596, -2.013242305049250280, 315.0000000000001137 ) ) ;
#1296 = CARTESIAN_POINT ( 'NONE',  ( -14.28417481768999941, 5.042936695466000430, -315.0848619657999734 ) ) ;
#1297 = DIRECTION ( 'NONE',  ( 0.000000000000000000, 0.000000000000000000, -1.000000000000000000 ) ) ;
#1298 = CARTESIAN_POINT ( 'NONE',  ( 18.35207017878000357, 4.220106527025000887, 320.0770942683900557 ) ) ;
#1299 = SURFACE_STYLE_USAGE ( .BOTH. , #10379 ) ;
#1300 = CARTESIAN_POINT ( 'NONE',  ( -0.6576834034345514501, -2.538582342225996769, -434.3791788602677570 ) ) ;
#1301 = VERTEX_POINT ( 'NONE', #6124 ) ;
#1302 = CARTESIAN_POINT ( 'NONE',  ( -18.93734960604998463, 3.176822791883000985, -317.5770954168139610 ) ) ;
#1303 = AXIS2_PLACEMENT_3D ( 'NONE', #4279, #7550, #441 ) ;
#1304 = CARTESIAN_POINT ( 'NONE',  ( 19.97263891460998764, 0.5563097477957001935, -316.3802825947000201 ) ) ;
#1305 = EDGE_CURVE ( 'NONE', #8275, #6555, #7638, .T. ) ;
#1306 = CARTESIAN_POINT ( 'NONE',  ( -51.72607275331812104, -12.50000000000000000, -370.6966883942067739 ) ) ;
#1307 = PLANE ( 'NONE',  #8112 ) ;
#1308 = EDGE_LOOP ( 'NONE', ( #7865, #5755, #3971, #875 ) ) ;
#1309 = CARTESIAN_POINT ( 'NONE',  ( -4.134979495079278422, -6.972766829544778666, -436.2920240787863690 ) ) ;
#1310 = CARTESIAN_POINT ( 'NONE',  ( -14.74684780783305449, -4.500000000000000888, -439.3959507452315165 ) ) ;
#1311 = EDGE_LOOP ( 'NONE', ( #3567, #5407, #5270, #3199 ) ) ;
#1312 = CARTESIAN_POINT ( 'NONE',  ( -12.03935733796000562, -9.983683518723006856, 191.1197171614399792 ) ) ;
#1313 = ORIENTED_EDGE ( 'NONE', *, *, #3388, .F. ) ;
#1314 = DIRECTION ( 'NONE',  ( 0.1071946444232958900, 0.000000000000000000, -0.9942380540931649024 ) ) ;
#1315 = CARTESIAN_POINT ( 'NONE',  ( 11.54867409098999964, -9.757628671089998207, -302.4229045757450081 ) ) ;
#1316 = CARTESIAN_POINT ( 'NONE',  ( 14.00000000000000000, 2.500000000000000000, -317.5000000000000000 ) ) ;
#1317 = CARTESIAN_POINT ( 'NONE',  ( -34.39269738225353024, -2.500000000000000000, -407.7262955260336525 ) ) ;
#1318 = CARTESIAN_POINT ( 'NONE',  ( -71.87348570190857799, -12.50000000000000000, -375.0609390264727949 ) ) ;
#1319 = CARTESIAN_POINT ( 'NONE',  ( -19.21835421908001607, -3.675208614194998447, 319.5792614743400009 ) ) ;
#1320 = CARTESIAN_POINT ( 'NONE',  ( -38.85901494634669007, -12.00000000000000000, -386.6556615250812570 ) ) ;
#1321 = CARTESIAN_POINT ( 'NONE',  ( -16.28527389671999970, 3.844447514156999812, 314.4150829855000211 ) ) ;
#1322 = VERTEX_POINT ( 'NONE', #178 ) ;
#1323 = CARTESIAN_POINT ( 'NONE',  ( -18.21004088691051948, -5.189404274100755110, 190.9999999999995737 ) ) ;
#1324 = AXIS2_PLACEMENT_3D ( 'NONE', #4265, #1079, #7534 ) ;
#1325 = CARTESIAN_POINT ( 'NONE',  ( -19.97284803234999018, -0.5555888903174002191, 318.8802828394900644 ) ) ;
#1326 = B_SPLINE_CURVE_WITH_KNOTS ( 'NONE', 3,
 ( #429, #10262, #8638, #3605 ),
 .UNSPECIFIED., .F., .F.,
 ( 4, 4 ),
 ( 0.000000000000000000, 1.000000000000000000 ),
 .UNSPECIFIED. ) ;
#1327 = FACE_OUTER_BOUND ( 'NONE', #5253, .T. ) ;
#1328 = ADVANCED_FACE ( 'NONE', ( #5111 ), #6816, .T. ) ;
#1329 = CARTESIAN_POINT ( 'NONE',  ( -19.00000000000000000, 0.000000000000000000, 190.0000000000100044 ) ) ;
#1330 = CARTESIAN_POINT ( 'NONE',  ( 0.000000000000000000, 10.00000000000000000, 315.0000000000000000 ) ) ;
#1331 = VECTOR ( 'NONE', #7819, 1000.000000000000000 ) ;
#1332 = CARTESIAN_POINT ( 'NONE',  ( 19.38368284813939013, -2.500000000000000000, -515.5999187775453265 ) ) ;
#1333 = CARTESIAN_POINT ( 'NONE',  ( -10.25126261553517537, 10.00000004282989785, 314.9999999999999432 ) ) ;
#1334 = CARTESIAN_POINT ( 'NONE',  ( -16.78721195431734614, -1.718634075882268908, -314.9999999999999432 ) ) ;
#1335 = CARTESIAN_POINT ( 'NONE',  ( -6.619999202174732034, -3.376841163498135234, -437.1676759332182769 ) ) ;
#1336 = CYLINDRICAL_SURFACE ( 'NONE', #1965, 15.00000000000002309 ) ;
#1337 = CARTESIAN_POINT ( 'NONE',  ( 11.71572875054933327, 12.50000000135959688, -316.5000000000000000 ) ) ;
#1338 = EDGE_CURVE ( 'NONE', #5915, #6684, #1, .T. ) ;
#1339 = CARTESIAN_POINT ( 'NONE',  ( 2.257099744627868443, 9.415190953705950605, -315.0000000000000568 ) ) ;
#1340 = CARTESIAN_POINT ( 'NONE',  ( 19.11670425725001010, 2.646693943201001264, 189.9229057364800042 ) ) ;
#1341 = CARTESIAN_POINT ( 'NONE',  ( -119.6503683519543983, -7.500000000000000000, -299.0840866897705155 ) ) ;
#1342 = EDGE_LOOP ( 'NONE', ( #4527, #6060, #10354, #3368 ) ) ;
#1343 = CARTESIAN_POINT ( 'NONE',  ( 6.052780067456072999, -4.500000000000000888, -524.2189112390747141 ) ) ;
#1344 = CARTESIAN_POINT ( 'NONE',  ( -78.52752440735136474, -2.500000000000000000, -384.5389737553005034 ) ) ;
#1345 = PRODUCT_CONTEXT ( 'NONE', #9633, 'mechanical' ) ;
#1346 = CARTESIAN_POINT ( 'NONE',  ( 4.578954556310520729, -9.145511589803685837, 315.0000000000000000 ) ) ;
#1347 = CARTESIAN_POINT ( 'NONE',  ( -13.24479143485999977, 5.858166912337999577, -315.0848619657999734 ) ) ;
#1348 = EDGE_CURVE ( 'NONE', #2010, #1489, #7829, .T. ) ;
#1349 = CARTESIAN_POINT ( 'NONE',  ( -9.425113983963564479, -8.435516021358374417, 314.4999463140480884 ) ) ;
#1350 = CARTESIAN_POINT ( 'NONE',  ( 19.38188031595998595, 1.781951755297001450, 320.0770942683900557 ) ) ;
#1351 = DIRECTION ( 'NONE',  ( -0.8820010751365675583, 0.000000000000000000, -0.4712473909295827323 ) ) ;
#1352 = CARTESIAN_POINT ( 'NONE',  ( -0.8844900259107285612, -2.565904207356001443, -434.5153608183709935 ) ) ;
#1353 = ORIENTED_EDGE ( 'NONE', *, *, #7256, .T. ) ;
#1354 = CARTESIAN_POINT ( 'NONE',  ( 19.60172830838999047, 0.3498260303710997721, -317.5770954168139610 ) ) ;
#1355 = CARTESIAN_POINT ( 'NONE',  ( -4.990336260259995882, -12.19640393417999036, -317.0792622552969533 ) ) ;
#1356 = AXIS2_PLACEMENT_3D ( 'NONE', #3266, #7300, #8854 ) ;
#1357 = CARTESIAN_POINT ( 'NONE',  ( 12.98706127646999953, -6.788989183774999603, -315.0000000000000000 ) ) ;
#1358 = PLANE ( 'NONE',  #3824 ) ;
#1359 = EDGE_LOOP ( 'NONE', ( #1930, #10581, #4963, #3339 ) ) ;
#1360 = CARTESIAN_POINT ( 'NONE',  ( -10.77777196380999847, 9.457622649256999026, 190.0000000000000000 ) ) ;
#1361 = AXIS2_PLACEMENT_3D ( 'NONE', #9213, #7589, #5809 ) ;
#1362 = CARTESIAN_POINT ( 'NONE',  ( -38.85901494634669007, -7.366296000000000177, -386.6556615250812570 ) ) ;
#1363 = ORIENTED_EDGE ( 'NONE', *, *, #977, .T. ) ;
#1364 = CARTESIAN_POINT ( 'NONE',  ( -79.31727611502927289, -2.500000000000000000, -351.2304352734219606 ) ) ;
#1365 = ORIENTED_EDGE ( 'NONE', *, *, #5468, .F. ) ;
#1366 = CARTESIAN_POINT ( 'NONE',  ( 1.669669261120717341, -9.454727574740482865, 315.0000000000000568 ) ) ;
#1367 = CARTESIAN_POINT ( 'NONE',  ( 1.652129430310999236, -12.05325387113999014, -302.4229045757450081 ) ) ;
#1368 = DIRECTION ( 'NONE',  ( 0.1247904863035892847, 0.000000000000000000, -0.9921831154218024862 ) ) ;
#1369 = CIRCLE ( 'NONE', #3267, 3.400000000000014122 ) ;
#1370 = CARTESIAN_POINT ( 'NONE',  ( -1.547234103168566133, -7.369705175477000658, -434.7990518850289163 ) ) ;
#1371 = CARTESIAN_POINT ( 'NONE',  ( -19.56025181625999920, -0.5259968871555997794, -302.4229045757450081 ) ) ;
#1372 = CARTESIAN_POINT ( 'NONE',  ( 20.00506338957998409, -0.1012955751877999966, 318.8802828394900644 ) ) ;
#1373 = VERTEX_POINT ( 'NONE', #1341 ) ;
#1374 = CARTESIAN_POINT ( 'NONE',  ( 3.971626792229000280, -9.186906450543000702, -315.0848619657999734 ) ) ;
#1375 = DIRECTION ( 'NONE',  ( -0.8820010751365678914, 0.000000000000000000, -0.4712473909295818442 ) ) ;
#1376 = VERTEX_POINT ( 'NONE', #8009 ) ;
#1377 = CARTESIAN_POINT ( 'NONE',  ( 19.37206517509000037, -1.821913627144001735, 189.9229057364800042 ) ) ;
#1378 = CARTESIAN_POINT ( 'NONE',  ( 3.204766135845001696, 12.34903855201999079, 318.8802828394900644 ) ) ;
#1379 = CIRCLE ( 'NONE', #9619, 3.400000000000014122 ) ;
#1380 = CARTESIAN_POINT ( 'NONE',  ( -86.86306229143158930, -2.500000000000000000, -370.6132103076870976 ) ) ;
#1381 = COLOUR_RGB ( '', 0.09019608, 0.27058824, 0.51372549) ;
#1382 = ORIENTED_EDGE ( 'NONE', *, *, #8963, .F. ) ;
#1383 = CARTESIAN_POINT ( 'NONE',  ( -1.257430124576000008, -9.427442400486999219, 315.0848619657999734 ) ) ;
#1384 = FACE_OUTER_BOUND ( 'NONE', #4703, .T. ) ;
#1385 = DIRECTION ( 'NONE',  ( 0.000000000000000000, 1.000000000000000000, 0.000000000000000000 ) ) ;
#1386 = CARTESIAN_POINT ( 'NONE',  ( -14.96969266857001557, -6.905075921034003805, 319.9928079742500131 ) ) ;
#1387 = CARTESIAN_POINT ( 'NONE',  ( -9.217250738626699302, -7.977707550455783725, -315.0000000000001137 ) ) ;
#1388 =( BOUNDED_CURVE ( )  B_SPLINE_CURVE ( 3, ( #590, #8321, #2631, #3325, #1008, #5955, #850, #7410, #1661, #2469, #6659, #4936, #4348, #6711, #5146, #8422, #4189, #9078, #2687, #5894, #1062, #9245, #6770, #9935, #5737, #8372, #9989, #1875, #7621, #8264, #956, #7568, #267, #1768, #8212, #213, #52, #157, #3544 ),
 .UNSPECIFIED., .F., .F. ) 
 B_SPLINE_CURVE_WITH_KNOTS ( ( 4, 1, 1, 1, 1, 1, 1, 1, 1, 1, 1, 1, 1, 1, 1, 1, 1, 1, 1, 1, 1, 1, 1, 1, 1, 1, 1, 1, 1, 1, 1, 1, 1, 1, 1, 1, 4 ),
 ( 0.000000000000000000, 0.03255837131920315264, 0.06556990764360211277, 0.09473136908033905068, 0.1200161462726948014, 0.1434330934855738426, 0.1672842806195496690, 0.1914679751100890059, 0.2155028411842019598, 0.2393474010340431446, 0.2632466635524260967, 0.2878286224669093785, 0.3134478398786056386, 0.3397600561265990970, 0.3667240395490956595, 0.3951494960372031184, 0.4259522906035831391, 0.4599907034545276385, 0.4966508108602696869, 0.5336723842619190972, 0.5687290606137788140, 0.6006810251919935117, 0.6302097713864018846, 0.6581574700887727891, 0.6853091452815192053, 0.7117521918490830046, 0.7371786555985279099, 0.7617219361653213561, 0.7857512081544899551, 0.8096666007474261351, 0.8337748265625606336, 0.8576111943424252759, 0.8809858201129860955, 0.9062047945899976975, 0.9352885204660792429, 0.9682251798361949380, 1.000000000000000000 ),
 .UNSPECIFIED. ) 
 CURVE ( )  GEOMETRIC_REPRESENTATION_ITEM ( )  RATIONAL_B_SPLINE_CURVE ( ( 1.171573374054913907, 1.171573374054913685, 1.171573374054913685, 1.171573374054913685, 1.171573374054913685, 1.171573374054913685, 1.171573374054913685, 1.171573374054913685, 1.171573374054913685, 1.171573374054913685, 1.171573374054913685, 1.171573374054913685, 1.171573374054913685, 1.171573374054913685, 1.171573374054913685, 1.171573374054913685, 1.171573374054913685, 1.171573374054913685, 1.171573374054913685, 1.171573374054913685, 1.171573374054913685, 1.171573374054913685, 1.171573374054913685, 1.171573374054913685, 1.171573374054913685, 1.171573374054913685, 1.171573374054913685, 1.171573374054913685, 1.171573374054913685, 1.171573374054913685, 1.171573374054913685, 1.171573374054913685, 1.171573374054913685, 1.171573374054913685, 1.171573374054913685, 1.171573374054913685, 1.171573374054913685, 1.171573374054913685, 1.171573374054913685 ) ) 
 REPRESENTATION_ITEM ( '' )  );
#1389 = DIRECTION ( 'NONE',  ( 0.9396926207858972147, 0.000000000000000000, 0.3420201433256990775 ) ) ;
#1390 = ORIENTED_EDGE ( 'NONE', *, *, #4717, .F. ) ;
#1391 = DIRECTION ( 'NONE',  ( -0.9712267471052594692, 0.000000000000000000, -0.2381566831044984178 ) ) ;
#1392 = AXIS2_PLACEMENT_3D ( 'NONE', #122, #8875, #3183 ) ;
#1393 = CARTESIAN_POINT ( 'NONE',  ( -8.691431531408321476, 8.152829611300951740, -315.0000000000000000 ) ) ;
#1394 = CARTESIAN_POINT ( 'NONE',  ( -20.04238130943000940, 0.9501178419093005978, 190.4207385301700128 ) ) ;
#1395 = CARTESIAN_POINT ( 'NONE',  ( 10.00000000000000000, -2.500000000000000000, -317.5000000000000000 ) ) ;
#1396 = VERTEX_POINT ( 'NONE', #1395 ) ;
#1397 = CARTESIAN_POINT ( 'NONE',  ( -13.35645252658000004, -8.162105094466999944, -317.5000000000000000 ) ) ;
#1398 = FACE_OUTER_BOUND ( 'NONE', #118, .T. ) ;
#1399 = PRODUCT_CONTEXT ( 'NONE', #1051, 'mechanical' ) ;
#1400 = CARTESIAN_POINT ( 'NONE',  ( 10.02519493912904380, -7.672398658596809362, 315.0000000000000568 ) ) ;
#1401 = CARTESIAN_POINT ( 'NONE',  ( -1.388768300183999882, 9.421618921053999784, -315.0848619657999734 ) ) ;
#1402 = DIRECTION ( 'NONE',  ( 0.000000000000000000, -1.000000000000000000, -0.000000000000000000 ) ) ;
#1403 = CIRCLE ( 'NONE', #3292, 15.50000000000001421 ) ;
#1404 = CARTESIAN_POINT ( 'NONE',  ( 20.05691220054001178, -0.5621708077868997622, 319.5792614743400009 ) ) ;
#1405 = PRESENTATION_STYLE_ASSIGNMENT (( #1299 ) ) ;
#1406 = CARTESIAN_POINT ( 'NONE',  ( -0.7175256489034935736, -2.498213111830998923, -434.1510992972750387 ) ) ;
#1407 = VERTEX_POINT ( 'NONE', #541 ) ;
#1408 = CARTESIAN_POINT ( 'NONE',  ( 12.61362476840000113, 9.241140244908006451, -317.5770954168139610 ) ) ;
#1409 = CARTESIAN_POINT ( 'NONE',  ( 20.01697452336999561, -0.3413909698088000710, -316.3802825947000201 ) ) ;
#1410 = EDGE_CURVE ( 'NONE', #1779, #9634, #8644, .T. ) ;
#1411 = AXIS2_PLACEMENT_3D ( 'NONE', #1089, #7596, #5176 ) ;
#1412 = CARTESIAN_POINT ( 'NONE',  ( -17.19853431800999743, -2.231396706187000145, -315.0000000000000000 ) ) ;
#1413 = EDGE_CURVE ( 'NONE', #9766, #8632, #588, .T. ) ;
#1414 = TOROIDAL_SURFACE ( 'NONE', #1935, 12.50000000000000000, 0.5000000000000000000 ) ;
#1415 = FACE_BOUND ( 'NONE', #6968, .T. ) ;
#1416 = VERTEX_POINT ( 'NONE', #7205 ) ;
#1417 = CARTESIAN_POINT ( 'NONE',  ( -15.54698342962807089, -4.499693933759679076, -314.5711572504542346 ) ) ;
#1418 = VERTEX_POINT ( 'NONE', #6174 ) ;
#1419 = FACE_OUTER_BOUND ( 'NONE', #4482, .T. ) ;
#1420 = ORIENTED_EDGE ( 'NONE', *, *, #7521, .T. ) ;
#1421 = CARTESIAN_POINT ( 'NONE',  ( -8.673721998911229747, -8.158754989085133857, 315.0000000000000568 ) ) ;
#1422 = CARTESIAN_POINT ( 'NONE',  ( -19.60176101890002442, -0.3495461351719001408, -302.4229045757450081 ) ) ;
#1423 = EDGE_CURVE ( 'NONE', #3853, #189, #8964, .T. ) ;
#1424 = CARTESIAN_POINT ( 'NONE',  ( -80.80421425739181984, -2.500000000000000000, -329.3491872523243842 ) ) ;
#1425 = CIRCLE ( 'NONE', #9488, 5.000000000000004441 ) ;
#1426 = EDGE_CURVE ( 'NONE', #10492, #1542, #5215, .T. ) ;
#1427 = CARTESIAN_POINT ( 'NONE',  ( 16.90094380520001849, 6.817658119454999444, -302.9207377450070453 ) ) ;
#1428 = DIRECTION ( 'NONE',  ( 0.000000000000000000, -1.000000000000000000, 0.000000000000000000 ) ) ;
#1429 = ORIENTED_EDGE ( 'NONE', *, *, #5752, .F. ) ;
#1430 = CARTESIAN_POINT ( 'NONE',  ( -10.32396869588999877, -7.471487098147999717, -315.0848619657999734 ) ) ;
#1431 = DIRECTION ( 'NONE',  ( -5.231093336277999443E-11, -3.356106971682999882E-12, 1.000000000000000000 ) ) ;
#1432 = ORIENTED_EDGE ( 'NONE', *, *, #6163, .F. ) ;
#1433 = CARTESIAN_POINT ( 'NONE',  ( 6.317945743273003956, -11.44290306353000730, 189.9229057364800042 ) ) ;
#1434 = CARTESIAN_POINT ( 'NONE',  ( -17.01113700077726776, 6.587853872568209646, 190.9999999999996589 ) ) ;
#1435 = CARTESIAN_POINT ( 'NONE',  ( -15.16362200326591569, -7.500000000000000000, -437.6963039377973246 ) ) ;
#1436 = EDGE_CURVE ( 'NONE', #7676, #4804, #4600, .T. ) ;
#1437 = ORIENTED_EDGE ( 'NONE', *, *, #3941, .F. ) ;
#1438 = CARTESIAN_POINT ( 'NONE',  ( -13.56771446467999986, -6.451120369226999607, 314.4150829855000211 ) ) ;
#1439 = CARTESIAN_POINT ( 'NONE',  ( -2.000000000000000000, 4.200000000000000178, -409.5000000000000000 ) ) ;
#1440 = CARTESIAN_POINT ( 'NONE',  ( 14.26294315260000012, 7.573769859179999564, 320.0000000000000000 ) ) ;
#1441 = CARTESIAN_POINT ( 'NONE',  ( -18.85507443398999428, -0.7700411122678003650, 319.9928079742500131 ) ) ;
#1442 = AXIS2_PLACEMENT_3D ( 'NONE', #2258, #3714, #7049 ) ;
#1443 = CARTESIAN_POINT ( 'NONE',  ( 19.96236207922240879, 0.9438262771025343056, 319.0000000000005116 ) ) ;
#1444 = CARTESIAN_POINT ( 'NONE',  ( -14.78164251960286890, -4.500000000000000000, -439.2540544344155933 ) ) ;
#1445 = CARTESIAN_POINT ( 'NONE',  ( 7.006889269069000115, 6.844138725329000472, 315.0000000000000000 ) ) ;
#1446 = AXIS2_PLACEMENT_3D ( 'NONE', #2951, #3606, #3652 ) ;
#1447 = ORIENTED_EDGE ( 'NONE', *, *, #3836, .F. ) ;
#1448 = CARTESIAN_POINT ( 'NONE',  ( -20.00000000000000000, -4.642018570833219964E-09, -303.5000000000000000 ) ) ;
#1449 = AXIS2_PLACEMENT_3D ( 'NONE', #2696, #4307, #9306 ) ;
#1450 = CLOSED_SHELL ( 'NONE', ( #6125, #6680, #4249, #152, #2598, #9705, #4681, #8027, #2131, #1291, #655, #6920, #4479, #4185, #3013, #3240, #637, #5572, #6836, #2413, #2799, #2213, #8047, #6176, #7498 ) ) ;
#1451 = CARTESIAN_POINT ( 'NONE',  ( -19.56033241475001816, -0.5267183861394004740, 189.9229057364800042 ) ) ;
#1452 = CARTESIAN_POINT ( 'NONE',  ( 16.24790196670450015, 3.755744802056943499, 314.4999487198771249 ) ) ;
#1453 = ORIENTED_EDGE ( 'NONE', *, *, #7309, .T. ) ;
#1454 = EDGE_CURVE ( 'NONE', #7492, #9535, #2957, .T. ) ;
#1455 = CARTESIAN_POINT ( 'NONE',  ( -20.00000000068207129, -7.322330470855613171, -303.4999999999999432 ) ) ;
#1456 = AXIS2_PLACEMENT_3D ( 'NONE', #3906, #7347, #5455 ) ;
#1457 = AXIS2_PLACEMENT_3D ( 'NONE', #5077, #10617, #4173 ) ;
#1458 = AXIS2_PLACEMENT_3D ( 'NONE', #8615, #2075, #6918 ) ;
#1459 = CARTESIAN_POINT ( 'NONE',  ( 11.84516230667378345, 6.793967159201454997, 315.0000000000000568 ) ) ;
#1460 = PRODUCT_CONTEXT ( 'NONE', #2761, 'mechanical' ) ;
#1461 = CARTESIAN_POINT ( 'NONE',  ( -10.54003729909880605, -10.63540770771157717, -303.4999999999996589 ) ) ;
#1462 = DIRECTION ( 'NONE',  ( 0.000000000000000000, -1.000000000000000000, 0.000000000000000000 ) ) ;
#1463 = DIRECTION ( 'NONE',  ( 0.000000000000000000, 1.000000000000000000, -0.000000000000000000 ) ) ;
#1464 = CARTESIAN_POINT ( 'NONE',  ( 12.03361782604000219, 9.527744202155000508, 320.0770942683900557 ) ) ;
#1465 = DIRECTION ( 'NONE',  ( 0.000000000000000000, -1.000000000000000000, 0.000000000000000000 ) ) ;
#1466 = CARTESIAN_POINT ( 'NONE',  ( -0.5984921290374501934, -2.530241314762997629, -434.3301463708660322 ) ) ;
#1467 = ORIENTED_EDGE ( 'NONE', *, *, #5835, .F. ) ;
#1468 = CARTESIAN_POINT ( 'NONE',  ( -10.62478234909000285, 10.68521885564000051, -317.0792622552969533 ) ) ;
#1469 = CARTESIAN_POINT ( 'NONE',  ( 17.73927626374001676, -5.796814996629003680, -316.3802825947000201 ) ) ;
#1470 = ADVANCED_FACE ( 'NONE', ( #3926 ), #5434, .T. ) ;
#1471 = EDGE_LOOP ( 'NONE', ( #1192, #1313, #4177, #3745 ) ) ;
#1472 = CARTESIAN_POINT ( 'NONE',  ( -17.35388116884000098, -4.663644590058999562, 320.0000000000000000 ) ) ;
#1473 = CARTESIAN_POINT ( 'NONE',  ( -0.5534908175310586653, -2.500000333914000006, -434.2941325283891274 ) ) ;
#1474 = DIRECTION ( 'NONE',  ( 0.000000000000000000, 0.000000000000000000, -1.000000000000000000 ) ) ;
#1475 = ORIENTED_EDGE ( 'NONE', *, *, #3973, .F. ) ;
#1476 = AXIS2_PLACEMENT_3D ( 'NONE', #2612, #5874, #3471 ) ;
#1477 = ADVANCED_FACE ( 'NONE', ( #4789 ), #7258, .F. ) ;
#1478 = CARTESIAN_POINT ( 'NONE',  ( 17.61684826078804278, -5.934684944789437644, 319.0000000000003979 ) ) ;
#1479 = ORIENTED_EDGE ( 'NONE', *, *, #6849, .F. ) ;
#1480 = DIRECTION ( 'NONE',  ( -0.8820010751365675583, 0.000000000000000000, -0.4712473909295827323 ) ) ;
#1481 = ORIENTED_EDGE ( 'NONE', *, *, #1562, .T. ) ;
#1482 =( BOUNDED_CURVE ( )  B_SPLINE_CURVE ( 3, ( #8611, #5240, #10132, #1156, #7813, #7714, #5658, #3895, #10443, #5549, #5443, #6255, #9752, #9588, #4059, #7174, #779, #4864, #3084, #10391, #1587, #8029, #3031, #9536, #6304, #9699, #8083, #2230, #2978, #674, #5497, #725, #2176, #6361, #4759, #7981, #2392, #8721, #9642 ),
 .UNSPECIFIED., .F., .F. ) 
 B_SPLINE_CURVE_WITH_KNOTS ( ( 4, 1, 1, 1, 1, 1, 1, 1, 1, 1, 1, 1, 1, 1, 1, 1, 1, 1, 1, 1, 1, 1, 1, 1, 1, 1, 1, 1, 1, 1, 1, 1, 1, 1, 1, 1, 4 ),
 ( 0.000000000000000000, 0.03177462182248489558, 0.06473445752888679072, 0.09385364856954797608, 0.1191010430400941816, 0.1424790257418306616, 0.1662901096498164977, 0.1904342604133075489, 0.2144298290992794898, 0.2382345388122185659, 0.2620932284128461021, 0.2866356387947041062, 0.3122179111685363662, 0.3384928023102437566, 0.3654153534982620410, 0.3937977678961499528, 0.4245599715672165320, 0.4585656223635951600, 0.4952131905531246825, 0.5322445193856788492, 0.5673324073471925910, 0.5993259174520088051, 0.6288994963735404786, 0.6568908825538778418, 0.6840816459652386827, 0.7105624348628037934, 0.7360296225686679961, 0.7606150911898691414, 0.7846847747132009721, 0.8086388669220148095, 0.8327860209783324308, 0.8566619651612987774, 0.8800749352578085549, 0.9053303401216608037, 0.9344548807899610843, 0.9674420121560727281, 1.000000000000000000 ),
 .UNSPECIFIED. ) 
 CURVE ( )  GEOMETRIC_REPRESENTATION_ITEM ( )  RATIONAL_B_SPLINE_CURVE ( ( 1.171573374019466041, 1.171573374019466263, 1.171573374019466041, 1.171573374019466263, 1.171573374019466263, 1.171573374019466263, 1.171573374019466263, 1.171573374019466263, 1.171573374019466263, 1.171573374019466263, 1.171573374019466263, 1.171573374019466263, 1.171573374019466263, 1.171573374019466263, 1.171573374019466263, 1.171573374019466263, 1.171573374019466263, 1.171573374019466263, 1.171573374019466263, 1.171573374019466263, 1.171573374019466263, 1.171573374019466263, 1.171573374019466263, 1.171573374019466263, 1.171573374019466263, 1.171573374019466263, 1.171573374019466263, 1.171573374019466263, 1.171573374019466263, 1.171573374019466263, 1.171573374019466263, 1.171573374019466263, 1.171573374019466263, 1.171573374019466263, 1.171573374019466263, 1.171573374019466263, 1.171573374019466263, 1.171573374019466263, 1.171573374019466263 ) ) 
 REPRESENTATION_ITEM ( '' )  );
#1483 = CARTESIAN_POINT ( 'NONE',  ( -10.54280934634114786, -7.451587612377529091, 315.0000000000000000 ) ) ;
#1484 = CARTESIAN_POINT ( 'NONE',  ( -11.53197558896999020, -9.764383963115998100, -302.4229045757450081 ) ) ;
#1485 = ADVANCED_FACE ( 'NONE', ( #9729 ), #3975, .T. ) ;
#1486 = CARTESIAN_POINT ( 'NONE',  ( -2.000000000003786749, -7.500000000000000888, -409.4999999999758415 ) ) ;
#1487 = CARTESIAN_POINT ( 'NONE',  ( -1.678162365823997915, 12.55068027652000140, -302.9207377450070453 ) ) ;
#1488 = CARTESIAN_POINT ( 'NONE',  ( 4.392607225559004291, -12.20457772578000366, 318.8802828394900644 ) ) ;
#1489 = VERTEX_POINT ( 'NONE', #10527 ) ;
#1490 = CARTESIAN_POINT ( 'NONE',  ( -12.21495827233999876, -7.290170534263999969, -314.4150829855000211 ) ) ;
#1491 = EDGE_CURVE ( 'NONE', #3141, #3262, #1508, .T. ) ;
#1492 = FACE_OUTER_BOUND ( 'NONE', #688, .T. ) ;
#1493 = ORIENTED_EDGE ( 'NONE', *, *, #432, .F. ) ;
#1494 = CARTESIAN_POINT ( 'NONE',  ( -13.35558048726000635, -8.018799577237007981, 190.0071920248299477 ) ) ;
#1495 = CARTESIAN_POINT ( 'NONE',  ( 18.71194885756699833, 4.439033925638975475, 190.9999999999996589 ) ) ;
#1496 = FACE_OUTER_BOUND ( 'NONE', #9347, .T. ) ;
#1497 = CARTESIAN_POINT ( 'NONE',  ( -6.322301096779000318, -8.991223814764000011, 314.8616023057000461 ) ) ;
#1498 = SURFACE_SIDE_STYLE ('',( #5574 ) ) ;
#1499 = CARTESIAN_POINT ( 'NONE',  ( -4.345375235838000449, 11.20786428128000090, 320.0000000000000000 ) ) ;
#1500 = CARTESIAN_POINT ( 'NONE',  ( 10.54985698513999637, -9.422913819601998142, 319.9928079742500131 ) ) ;
#1501 = CARTESIAN_POINT ( 'NONE',  ( -16.30951479290585837, 7.248637510199256617, 319.0000000000005116 ) ) ;
#1502 = CARTESIAN_POINT ( 'NONE',  ( -14.85178883355849599, -4.396734861472281430, -438.9679907580307940 ) ) ;
#1503 = CARTESIAN_POINT ( 'NONE',  ( 16.90189876424999937, -0.3838616842170000099, 315.0848619657999734 ) ) ;
#1504 = ORIENTED_EDGE ( 'NONE', *, *, #2729, .T. ) ;
#1505 = CARTESIAN_POINT ( 'NONE',  ( -72.90663470102438737, 7.399494936611693774, -371.7168990826883714 ) ) ;
#1506 = PRODUCT_DEFINITION_SHAPE ( 'NONE', 'NONE',  #2191 ) ;
#1507 = CARTESIAN_POINT ( 'NONE',  ( 18.35205128653998230, 4.220047386950002810, 189.9229057364800042 ) ) ;
#1508 = LINE ( 'NONE', #8502, #7111 ) ;
#1509 = ORIENTED_EDGE ( 'NONE', *, *, #6127, .T. ) ;
#1510 = VECTOR ( 'NONE', #8979, 1000.000000000000000 ) ;
#1511 = LINE ( 'NONE', #4035, #8370 ) ;
#1512 = CARTESIAN_POINT ( 'NONE',  ( 14.02825138570089081, 5.340904894142199488, 315.0000000000000568 ) ) ;
#1513 = APPLICATION_PROTOCOL_DEFINITION ( 'draft international standard', 'automotive_design', 1998, #5641 ) ;
#1514 = CARTESIAN_POINT ( 'NONE',  ( -84.02975002432511076, -2.500000000000000000, -342.4104245220563030 ) ) ;
#1515 = CARTESIAN_POINT ( 'NONE',  ( -17.62021515802999971, -4.315182425209999728, -302.4999999999969873 ) ) ;
#1516 = CARTESIAN_POINT ( 'NONE',  ( -18.75085780967000559, 3.496151560526002289, 320.0770942683900557 ) ) ;
#1517 = CYLINDRICAL_SURFACE ( 'NONE', #2762, 3.499999999999999556 ) ;
#1518 = CARTESIAN_POINT ( 'NONE',  ( -1.668977462971013681, -2.537472099014000726, -434.6413441610087034 ) ) ;
#1519 = VERTEX_POINT ( 'NONE', #9321 ) ;
#1520 = CARTESIAN_POINT ( 'NONE',  ( -19.60211473220001110, 0.3233313581039002904, -317.5770954168139610 ) ) ;
#1521 = DIRECTION ( 'NONE',  ( -0.000000000000000000, 1.000000000000000000, 0.000000000000000000 ) ) ;
#1522 = CARTESIAN_POINT ( 'NONE',  ( 7.333949653644999955, -10.60950709473999964, 320.0000000000000000 ) ) ;
#1523 = DIRECTION ( 'NONE',  ( 0.000000000000000000, 1.000000000000000000, 0.000000000000000000 ) ) ;
#1524 = CARTESIAN_POINT ( 'NONE',  ( 16.99964540243389521, -0.4333634660859933541, -315.0000000000000000 ) ) ;
#1525 = EDGE_LOOP ( 'NONE', ( #4822, #7801, #3032, #3409 ) ) ;
#1526 = CARTESIAN_POINT ( 'NONE',  ( 13.88765719697804180, -9.006220412848989554, 319.0000000000003979 ) ) ;
#1527 = EDGE_CURVE ( 'NONE', #9271, #890, #5926, .T. ) ;
#1528 = EDGE_LOOP ( 'NONE', ( #5275, #7312, #1559, #3644, #3139, #4760, #5881, #4377, #9229 ) ) ;
#1529 = LINE ( 'NONE', #564, #1934 ) ;
#1530 = VERTEX_POINT ( 'NONE', #5273 ) ;
#1531 = CARTESIAN_POINT ( 'NONE',  ( -2.737043330023148258, -9.374968016864249520, 315.0000000000000568 ) ) ;
#1532 = CARTESIAN_POINT ( 'NONE',  ( -8.052748353536003378, -11.53355103076000532, -302.9207377450070453 ) ) ;
#1533 = CARTESIAN_POINT ( 'NONE',  ( -30.87192209819000155, 2.500000000000000000, -461.0868123482000556 ) ) ;
#1534 = CARTESIAN_POINT ( 'NONE',  ( -2.000000000000000000, -9.500000000000000000, -413.0000000000000000 ) ) ;
#1535 = ADVANCED_FACE ( 'NONE', ( #10169 ), #9270, .T. ) ;
#1536 = SURFACE_STYLE_FILL_AREA ( #6642 ) ;
#1537 = EDGE_CURVE ( 'NONE', #2499, #8275, #10201, .T. ) ;
#1538 = AXIS2_PLACEMENT_3D ( 'NONE', #6704, #5030, #7508 ) ;
#1539 = VECTOR ( 'NONE', #4099, 1000.000000000000000 ) ;
#1540 = CARTESIAN_POINT ( 'NONE',  ( 11.53197558896999020, 9.764383963115998100, -302.4229045757450081 ) ) ;
#1541 = CARTESIAN_POINT ( 'NONE',  ( 6.038923639677001631, -11.92375595181999870, 318.8802828394900644 ) ) ;
#1542 = VERTEX_POINT ( 'NONE', #6029 ) ;
#1543 = CARTESIAN_POINT ( 'NONE',  ( 6.388932193737000276, -8.746770244069999478, -315.0848619657999734 ) ) ;
#1544 = DIRECTION ( 'NONE',  ( 0.9902680687415800209, 0.000000000000000000, 0.1391731009599966873 ) ) ;
#1545 = ORIENTED_EDGE ( 'NONE', *, *, #9391, .T. ) ;
#1546 = CARTESIAN_POINT ( 'NONE',  ( 19.56033241475001816, 0.5267183861393005539, 189.9229057364800042 ) ) ;
#1547 = CARTESIAN_POINT ( 'NONE',  ( -80.80421425739181984, -7.500000000000000000, -329.3491872523243842 ) ) ;
#1548 = CARTESIAN_POINT ( 'NONE',  ( 10.00000000000000000, 2.500000000000000000, -317.5000000000000000 ) ) ;
#1549 = VECTOR ( 'NONE', #3392, 1000.000000000000000 ) ;
#1550 = EDGE_CURVE ( 'NONE', #2509, #9430, #5096, .T. ) ;
#1551 = CARTESIAN_POINT ( 'NONE',  ( -10.32396869588999877, -7.471487098147999717, 315.0848619657999734 ) ) ;
#1552 =( NAMED_UNIT ( * ) PLANE_ANGLE_UNIT ( ) SI_UNIT ( $, .RADIAN. ) );
#1553 = EDGE_CURVE ( 'NONE', #471, #9652, #10117, .T. ) ;
#1554 = CARTESIAN_POINT ( 'NONE',  ( -20.57979856674000629, -2.500000000000000000, -389.8948508258000061 ) ) ;
#1555 = DIRECTION ( 'NONE',  ( 0.000000000000000000, 1.000000000000000000, 0.000000000000000000 ) ) ;
#1556 = LINE ( 'NONE', #8003, #4345 ) ;
#1557 = CARTESIAN_POINT ( 'NONE',  ( -1.514431797236434930E-09, -10.00000000000000000, -302.4999999999999432 ) ) ;
#1558 = DIRECTION ( 'NONE',  ( 0.5828070674935411644, 0.000000000000000000, 0.8126105599114368250 ) ) ;
#1559 = ORIENTED_EDGE ( 'NONE', *, *, #4277, .T. ) ;
#1560 = CARTESIAN_POINT ( 'NONE',  ( -2.000000000003786749, -7.500000000000000888, -409.4999999999758415 ) ) ;
#1561 = ORIENTED_EDGE ( 'NONE', *, *, #568, .T. ) ;
#1562 = EDGE_CURVE ( 'NONE', #320, #8561, #2812, .T. ) ;
#1563 = ORIENTED_EDGE ( 'NONE', *, *, #9381, .F. ) ;
#1564 = CARTESIAN_POINT ( 'NONE',  ( -51.41224207513210587, -8.000000000000000000, -371.0859316413305464 ) ) ;
#1565 = CARTESIAN_POINT ( 'NONE',  ( -17.16660215780892784, -1.253874176888070540E-08, -314.8332688233516024 ) ) ;
#1566 =( LENGTH_UNIT ( ) NAMED_UNIT ( * ) SI_UNIT ( .MILLI., .METRE. ) );
#1567 = CARTESIAN_POINT ( 'NONE',  ( 18.56827417761491361, -4.704550062028092228, -303.4999999999996589 ) ) ;
#1568 = CARTESIAN_POINT ( 'NONE',  ( -10.18931492271999950, -9.698324433322001781, -302.5000000000000000 ) ) ;
#1569 = CARTESIAN_POINT ( 'NONE',  ( -2.000000000000000000, 2.500000000000000000, -409.5000000000000000 ) ) ;
#1570 = DIRECTION ( 'NONE',  ( 0.000000000000000000, 1.000000000000000000, 0.000000000000000000 ) ) ;
#1571 = CARTESIAN_POINT ( 'NONE',  ( -17.67524584885999772, 5.985122643679996912, 319.5792614743400009 ) ) ;
#1572 = CARTESIAN_POINT ( 'NONE',  ( 14.00000000000000000, 2.500000000000000000, -410.4979246179000256 ) ) ;
#1573 = CARTESIAN_POINT ( 'NONE',  ( 13.57573464316000056, 3.225916527208000151, 315.0000000000001705 ) ) ;
#1574 = EDGE_LOOP ( 'NONE', ( #5986, #3411, #10416, #5487 ) ) ;
#1575 = CARTESIAN_POINT ( 'NONE',  ( -19.98286815278001427, -0.4166756924005995955, -316.3802825947000201 ) ) ;
#1576 = CARTESIAN_POINT ( 'NONE',  ( -0.1454145850583489497, -8.513384478312998382, -435.8155006440865691 ) ) ;
#1577 = EDGE_CURVE ( 'NONE', #3224, #9652, #4271, .T. ) ;
#1578 = ORIENTED_EDGE ( 'NONE', *, *, #8707, .F. ) ;
#1579 = CARTESIAN_POINT ( 'NONE',  ( 17.34782881681000077, -4.671787541421999812, 320.0000000000000000 ) ) ;
#1580 = CARTESIAN_POINT ( 'NONE',  ( -0.4619277171041915042, -7.556499546952999857, -434.7365042083650906 ) ) ;
#1581 = CIRCLE ( 'NONE', #2784, 0.5000000000000004441 ) ;
#1582 = DIRECTION ( 'NONE',  ( -0.9712267471052612455, 0.000000000000000000, -0.2381566831044910626 ) ) ;
#1583 = FACE_OUTER_BOUND ( 'NONE', #10228, .T. ) ;
#1584 = VERTEX_POINT ( 'NONE', #500 ) ;
#1585 = CARTESIAN_POINT ( 'NONE',  ( 19.99997414083856739, -0.3194320646935533969, 319.0000000000003979 ) ) ;
#1586 = ORIENTED_EDGE ( 'NONE', *, *, #7520, .F. ) ;
#1587 = CARTESIAN_POINT ( 'NONE',  ( 1.602145841528213932, 12.47735433440135644, -316.5000000000004547 ) ) ;
#1588 = ORIENTED_EDGE ( 'NONE', *, *, #1491, .F. ) ;
#1589 = CARTESIAN_POINT ( 'NONE',  ( 0.9841565935054803482, -9.488387273935385835, 314.9999999999999432 ) ) ;
#1590 = CARTESIAN_POINT ( 'NONE',  ( 19.31742247159998271, -3.345204157467998929, -303.6197174156509391 ) ) ;
#1591 = CYLINDRICAL_SURFACE ( 'NONE', #6329, 3.500000000000020428 ) ;
#1592 = AXIS2_PLACEMENT_3D ( 'NONE', #4702, #621, #6470 ) ;
#1593 = VECTOR ( 'NONE', #8757, 1000.000000000000000 ) ;
#1594 = DIRECTION ( 'NONE',  ( -0.2951854283188012906, 0.000000000000000000, 0.9554399839384188908 ) ) ;
#1595 = EDGE_CURVE ( 'NONE', #5654, #6416, #2475, .T. ) ;
#1596 =( NAMED_UNIT ( * ) SI_UNIT ( $, .STERADIAN. ) SOLID_ANGLE_UNIT ( ) );
#1597 = CARTESIAN_POINT ( 'NONE',  ( 3.644643686525998572, 11.88155656384000203, -302.4229045757450081 ) ) ;
#1598 = CARTESIAN_POINT ( 'NONE',  ( 13.88394749849000043, -9.000054837070988967, 318.8802828394900644 ) ) ;
#1599 = ORIENTED_EDGE ( 'NONE', *, *, #3133, .T. ) ;
#1600 = CARTESIAN_POINT ( 'NONE',  ( -1.276003512426000075, -9.874146089817999794, -314.6383426456000052 ) ) ;
#1601 = CARTESIAN_POINT ( 'NONE',  ( 16.13341719193999779, 6.058597787994999706, -302.5000000000000000 ) ) ;
#1602 = CIRCLE ( 'NONE', #8454, 29.99999999999998224 ) ;
#1603 = ORIENTED_EDGE ( 'NONE', *, *, #9616, .T. ) ;
#1604 = CARTESIAN_POINT ( 'NONE',  ( -17.75414941409001557, -3.856242593410000197, 190.0071920248299477 ) ) ;
#1605 = LINE ( 'NONE', #4877, #3330 ) ;
#1606 = CARTESIAN_POINT ( 'NONE',  ( -13.64075175739777102, 5.653800323622448332, -315.0000000000000568 ) ) ;
#1607 = CARTESIAN_POINT ( 'NONE',  ( -83.90876261087991850, -7.500000000000000000, -346.8809236044617137 ) ) ;
#1608 = CARTESIAN_POINT ( 'NONE',  ( -14.52969073417999901, -5.422537850045999974, 314.6383426456000052 ) ) ;
#1609 =( NAMED_UNIT ( * ) SI_UNIT ( $, .STERADIAN. ) SOLID_ANGLE_UNIT ( ) );
#1610 = CARTESIAN_POINT ( 'NONE',  ( -16.83239583074999857, 5.311267823799999732, 320.0000000000000000 ) ) ;
#1611 = FACE_BOUND ( 'NONE', #3102, .T. ) ;
#1612 = CARTESIAN_POINT ( 'NONE',  ( 17.65399305443192901, 5.890951312620557268, 319.0000000000005116 ) ) ;
#1613 =( NAMED_UNIT ( * ) PLANE_ANGLE_UNIT ( ) SI_UNIT ( $, .RADIAN. ) );
#1614 = CARTESIAN_POINT ( 'NONE',  ( 15.00000000000000000, 0.4945770392355999800, 315.0000000000000000 ) ) ;
#1615 = ORIENTED_EDGE ( 'NONE', *, *, #1024, .T. ) ;
#1616 = CARTESIAN_POINT ( 'NONE',  ( 13.57573464316000056, 3.225916527208000151, -285.0000000000000000 ) ) ;
#1617 = ADVANCED_FACE ( 'NONE', ( #2164 ), #2915, .T. ) ;
#1618 = AXIS2_PLACEMENT_3D ( 'NONE', #2125, #4595, #5289 ) ;
#1619 = PLANE ( 'NONE',  #3401 ) ;
#1620 = FACE_OUTER_BOUND ( 'NONE', #6632, .T. ) ;
#1621 = CIRCLE ( 'NONE', #7626, 3.499999999999999556 ) ;
#1622 = CARTESIAN_POINT ( 'NONE',  ( -1.984036549750167078, -12.45525792938212284, -303.4999999999996589 ) ) ;
#1623 = CARTESIAN_POINT ( 'NONE',  ( 17.34089965840999881, 0.6440164457022999889, -314.6383426456000052 ) ) ;
#1624 = CARTESIAN_POINT ( 'NONE',  ( -14.96977070983867009, -9.000000000000001776, -385.2505660326773409 ) ) ;
#1625 =( NAMED_UNIT ( * ) PLANE_ANGLE_UNIT ( ) SI_UNIT ( $, .RADIAN. ) );
#1626 = CARTESIAN_POINT ( 'NONE',  ( -1.486103177728019809, -2.642483842335999089, -435.2287432255328667 ) ) ;
#1627 = FACE_OUTER_BOUND ( 'NONE', #4357, .T. ) ;
#1628 = CARTESIAN_POINT ( 'NONE',  ( -0.2363117521398999110, 12.51008298726001300, -316.3802825947000201 ) ) ;
#1629 = DIRECTION ( 'NONE',  ( -0.9921831154218024862, 0.000000000000000000, -0.1247904863035890766 ) ) ;
#1630 = VECTOR ( 'NONE', #3515, 1000.000000000000000 ) ;
#1631 = CIRCLE ( 'NONE', #1276, 5.000000000000008882 ) ;
#1632 = CARTESIAN_POINT ( 'NONE',  ( -16.84305512206999822, -5.298470530761999697, 320.0000000000000000 ) ) ;
#1633 = CARTESIAN_POINT ( 'NONE',  ( -0.5253760780244931539, -7.541458695310001126, -434.7805624543377689 ) ) ;
#1634 = UNCERTAINTY_MEASURE_WITH_UNIT (LENGTH_MEASURE( 1.000000000000000082E-05 ), #4296, 'distance_accuracy_value', 'NONE');
#1635 = DIRECTION ( 'NONE',  ( -0.000000000000000000, 1.000000000000000000, 0.000000000000000000 ) ) ;
#1636 = CARTESIAN_POINT ( 'NONE',  ( 16.39029893813008343, -2.501810464458257943, -315.0000000000000568 ) ) ;
#1637 = ORIENTED_EDGE ( 'NONE', *, *, #8378, .T. ) ;
#1638 = CARTESIAN_POINT ( 'NONE',  ( 6.348506474365276375, -9.305625771097021826, -314.5281326612879411 ) ) ;
#1639 = ORIENTED_EDGE ( 'NONE', *, *, #5745, .F. ) ;
#1640 = DIRECTION ( 'NONE',  ( 0.000000000000000000, 0.000000000000000000, 1.000000000000000000 ) ) ;
#1641 = ORIENTED_EDGE ( 'NONE', *, *, #8707, .T. ) ;
#1642 = CARTESIAN_POINT ( 'NONE',  ( 20.01694242003000568, -0.3416920405409001327, -303.6197174156509391 ) ) ;
#1643 = CARTESIAN_POINT ( 'NONE',  ( -82.18980308971114823, -7.500000000000000000, -388.2946789300659134 ) ) ;
#1644 = DIRECTION ( 'NONE',  ( 0.9936574763089274231, 0.000000000000000000, 0.1124491875265153373 ) ) ;
#1645 = CARTESIAN_POINT ( 'NONE',  ( -12.89386942443999295, 9.656754267509002787, -302.9207377450070453 ) ) ;
#1646 = CARTESIAN_POINT ( 'NONE',  ( -17.49999996772987743, -5.857864456328762515, 314.4997059534069308 ) ) ;
#1647 = EDGE_LOOP ( 'NONE', ( #8599, #7824, #2420, #5607 ) ) ;
#1648 = DIRECTION ( 'NONE',  ( -0.000000000000000000, 1.000000000000000000, 0.000000000000000000 ) ) ;
#1649 = CARTESIAN_POINT ( 'NONE',  ( 7.774319915545000015, 10.49237824600999858, -302.5000000000000000 ) ) ;
#1650 = ORIENTED_EDGE ( 'NONE', *, *, #2610, .F. ) ;
#1651 = CARTESIAN_POINT ( 'NONE',  ( -10.00032506892000406, -10.91649673191999526, 190.4207385301700128 ) ) ;
#1652 = DIRECTION ( 'NONE',  ( -0.1071946444232959594, 0.000000000000000000, 0.9942380540931649024 ) ) ;
#1653 = CARTESIAN_POINT ( 'NONE',  ( 13.95711901494857443, 5.398584340276486593, -315.0000000000000568 ) ) ;
#1654 = DIRECTION ( 'NONE',  ( 0.000000000000000000, -1.000000000000000000, 0.000000000000000000 ) ) ;
#1655 = EDGE_LOOP ( 'NONE', ( #322, #8238, #1851, #243 ) ) ;
#1656 = CARTESIAN_POINT ( 'NONE',  ( 17.21448334449999962, -1.351716521078000222, 314.6383426456000052 ) ) ;
#1657 =( LENGTH_UNIT ( ) NAMED_UNIT ( * ) SI_UNIT ( .MILLI., .METRE. ) );
#1658 = CARTESIAN_POINT ( 'NONE',  ( -17.34782881681000077, 4.671787541421999812, 320.0000000000000000 ) ) ;
#1659 = CARTESIAN_POINT ( 'NONE',  ( 7.392698694382005442, -11.19283382348000622, 320.0770942683900557 ) ) ;
#1660 = CARTESIAN_POINT ( 'NONE',  ( -9.914941699848355938, 10.86515064494810545, 319.0000000000005116 ) ) ;
#1661 = CARTESIAN_POINT ( 'NONE',  ( 14.92864611359688531, 8.336576156742356858, -303.4999999999990905 ) ) ;
#1662 = FACE_BOUND ( 'NONE', #3043, .T. ) ;
#1663 = ORIENTED_EDGE ( 'NONE', *, *, #407, .T. ) ;
#1664 = DIRECTION ( 'NONE',  ( 0.000000000000000000, -0.7071067811864661934, -0.7071067811866287300 ) ) ;
#1665 =( REPRESENTATION_RELATIONSHIP ('NONE','NONE', #8468, #7381 ) REPRESENTATION_RELATIONSHIP_WITH_TRANSFORMATION ( #2639 )SHAPE_REPRESENTATION_RELATIONSHIP( ) );
#1666 = AXIS2_PLACEMENT_3D ( 'NONE', #10062, #333, #3610 ) ;
#1667 = ADVANCED_FACE ( 'NONE', ( #2269 ), #5535, .T. ) ;
#1668 = EDGE_CURVE ( 'NONE', #1962, #3427, #7061, .T. ) ;
#1669 = CYLINDRICAL_SURFACE ( 'NONE', #557, 2.000000000000003997 ) ;
#1670 = DIRECTION ( 'NONE',  ( 0.000000000000000000, 0.000000000000000000, -1.000000000000000000 ) ) ;
#1671 = EDGE_CURVE ( 'NONE', #9606, #10567, #2305, .T. ) ;
#1672 = CARTESIAN_POINT ( 'NONE',  ( 16.90189876424999937, -0.3838616842170000099, -315.0848619657999734 ) ) ;
#1673 = CARTESIAN_POINT ( 'NONE',  ( -20.57979856674000629, 2.500000000000000000, -389.8948508258000061 ) ) ;
#1674 = DIRECTION ( 'NONE',  ( 0.9712269959794516128, -1.472254293302932272E-12, 0.2381556681683856258 ) ) ;
#1675 = CARTESIAN_POINT ( 'NONE',  ( -72.90663470102438737, -12.50000000000000000, -371.7168990826883714 ) ) ;
#1676 = CARTESIAN_POINT ( 'NONE',  ( 11.28781796570999951, 4.951468039558000633, 315.0000000000001705 ) ) ;
#1677 = ORIENTED_EDGE ( 'NONE', *, *, #10150, .F. ) ;
#1678 = AXIS2_PLACEMENT_3D ( 'NONE', #9635, #3832, #396 ) ;
#1679 = CARTESIAN_POINT ( 'NONE',  ( -17.73927626374001676, 5.796814996629003680, -316.3802825947000201 ) ) ;
#1680 = EDGE_LOOP ( 'NONE', ( #8671, #5541, #1588, #1899 ) ) ;
#1681 = CARTESIAN_POINT ( 'NONE',  ( -18.20902923167000154, -3.282017551273999967, 320.0000000000000000 ) ) ;
#1682 = EDGE_CURVE ( 'NONE', #9271, #722, #5114, .T. ) ;
#1683 = CARTESIAN_POINT ( 'NONE',  ( -0.1066158053962373981, -7.660711547938000798, -434.1593156514779253 ) ) ;
#1684 = AXIS2_PLACEMENT_3D ( 'NONE', #10257, #2846, #2193 ) ;
#1685 = CYLINDRICAL_SURFACE ( 'NONE', #3076, 1.999999999999998224 ) ;
#1686 = CARTESIAN_POINT ( 'NONE',  ( 4.648899539349734766, -9.134382686408038410, -315.0000000000001137 ) ) ;
#1687 = ORIENTED_EDGE ( 'NONE', *, *, #5354, .F. ) ;
#1688 = CARTESIAN_POINT ( 'NONE',  ( -17.19853431801041665, 2.231396706186351775, -315.0000000000001137 ) ) ;
#1689 = VERTEX_POINT ( 'NONE', #3721 ) ;
#1690 = DIRECTION ( 'NONE',  ( 0.1071946444232947937, 0.000000000000000000, -0.9942380540931651245 ) ) ;
#1691 = EDGE_LOOP ( 'NONE', ( #7871, #8545, #2831, #240 ) ) ;
#1692 = CARTESIAN_POINT ( 'NONE',  ( 19.39478698591998551, -3.379789856048000196, -302.9207377450070453 ) ) ;
#1693 = CARTESIAN_POINT ( 'NONE',  ( 18.86306334786000605, 0.4771235332119000971, -317.4928077629770087 ) ) ;
#1694 = EDGE_CURVE ( 'NONE', #7772, #4372, #1906, .T. ) ;
#1695 = MANIFOLD_SOLID_BREP ( 'Stock-MAS-686-1', #6776 ) ;
#1696 = PLANE ( 'NONE',  #3521 ) ;
#1697 = PRESENTATION_STYLE_ASSIGNMENT (( #6532 ) ) ;
#1698 = CARTESIAN_POINT ( 'NONE',  ( 9.312701725069002734, 11.06649994634999246, -303.6197174156509391 ) ) ;
#1699 = CARTESIAN_POINT ( 'NONE',  ( -10.00000000000000000, -2.500000000000000000, -317.5000000000000000 ) ) ;
#1700 = ORIENTED_EDGE ( 'NONE', *, *, #9251, .F. ) ;
#1701 = CARTESIAN_POINT ( 'NONE',  ( -82.14476046060677561, -2.500000000000000000, -345.9384288226025888 ) ) ;
#1702 = CARTESIAN_POINT ( 'NONE',  ( -69.81963093799060971, -7.500000000000000000, -370.0675332144908793 ) ) ;
#1703 = ORIENTED_EDGE ( 'NONE', *, *, #9636, .T. ) ;
#1704 = CARTESIAN_POINT ( 'NONE',  ( -20.08919666923998903, -0.07462331497648995449, 190.4207385301700128 ) ) ;
#1705 = CARTESIAN_POINT ( 'NONE',  ( 17.50000000000126832, -0.7437989020612977287, -314.4944826805096341 ) ) ;
#1706 = CARTESIAN_POINT ( 'NONE',  ( 16.34919249956382714, 2.583378889817198765, -314.9999999999999432 ) ) ;
#1707 = CYLINDRICAL_SURFACE ( 'NONE', #5477, 10.00000000000000000 ) ;
#1708 = CARTESIAN_POINT ( 'NONE',  ( -6.420662313211997763, 11.93024803506000531, 190.4207385301700128 ) ) ;
#1709 = AXIS2_PLACEMENT_3D ( 'NONE', #18, #1523, #3137 ) ;
#1710 = VECTOR ( 'NONE', #4006, 1000.000000000000000 ) ;
#1711 = EDGE_CURVE ( 'NONE', #4107, #7563, #6183, .T. ) ;
#1712 = CARTESIAN_POINT ( 'NONE',  ( 17.56758064089999749, -0.6313722887073999201, 314.4150829855000211 ) ) ;
#1713 = DIRECTION ( 'NONE',  ( 0.000000000000000000, 0.000000000000000000, -1.000000000000000000 ) ) ;
#1714 = CARTESIAN_POINT ( 'NONE',  ( 19.54690800120000205, -0.8885403386512999990, 320.0770942683900557 ) ) ;
#1715 = LINE ( 'NONE', #4987, #9837 ) ;
#1716 = CARTESIAN_POINT ( 'NONE',  ( 10.58801790939999954, 8.088125079530000150, 314.4150829855000211 ) ) ;
#1717 = VERTEX_POINT ( 'NONE', #3883 ) ;
#1718 = CARTESIAN_POINT ( 'NONE',  ( -78.09771732525952359, -7.500000000000000000, -330.1706946207383453 ) ) ;
#1719 = ORIENTED_EDGE ( 'NONE', *, *, #10081, .T. ) ;
#1720 = ORIENTED_EDGE ( 'NONE', *, *, #1454, .F. ) ;
#1721 = VECTOR ( 'NONE', #836, 1000.000000000000000 ) ;
#1722 = CARTESIAN_POINT ( 'NONE',  ( -1.723815153757401353, -2.911508528774001459, -435.2348705281305001 ) ) ;
#1723 = CIRCLE ( 'NONE', #7116, 3.500000000000003109 ) ;
#1724 = CARTESIAN_POINT ( 'NONE',  ( 2.450606348566487735, 9.399923241459493539, 315.0000000000000568 ) ) ;
#1725 = CONTEXT_DEPENDENT_SHAPE_REPRESENTATION ( #4007, #6906 ) ;
#1726 = DIRECTION ( 'NONE',  ( 0.9554399839384175586, 0.000000000000000000, 0.2951854283188048989 ) ) ;
#1727 = ORIENTED_EDGE ( 'NONE', *, *, #8494, .F. ) ;
#1728 = CARTESIAN_POINT ( 'NONE',  ( -0.6577138333327989805, -2.500183709831155454, -434.1612907480973149 ) ) ;
#1729 = SURFACE_SIDE_STYLE ('',( #3344 ) ) ;
#1730 = DIRECTION ( 'NONE',  ( 0.000000000000000000, 1.000000000000000000, -0.000000000000000000 ) ) ;
#1731 = PLANE ( 'NONE',  #595 ) ;
#1732 = CARTESIAN_POINT ( 'NONE',  ( -3.762811461229003562, 12.28417267642999278, -316.3802825947000201 ) ) ;
#1733 = PRODUCT_RELATED_PRODUCT_CATEGORY ( 'part', '', ( #1924 ) ) ;
#1734 = DIRECTION ( 'NONE',  ( -0.2951854283188049544, 0.000000000000000000, 0.9554399839384176696 ) ) ;
#1735 = CARTESIAN_POINT ( 'NONE',  ( -1.121771287418490415, -7.384865809656000479, -434.8579640789354244 ) ) ;
#1736 = DIRECTION ( 'NONE',  ( 0.000000000000000000, -1.000000000000000000, 0.000000000000000000 ) ) ;
#1737 = CARTESIAN_POINT ( 'NONE',  ( 16.37727794820371940, -2.527950228764472396, -315.0000000000001137 ) ) ;
#1738 = VERTEX_POINT ( 'NONE', #7855 ) ;
#1739 = SHAPE_REPRESENTATION ( 'Secondary Linkage Connector', ( #2817 ), #4734 ) ;
#1740 = DIRECTION ( 'NONE',  ( 0.000000000000000000, 1.000000000000000000, 0.000000000000000000 ) ) ;
#1741 = EDGE_LOOP ( 'NONE', ( #6927, #2531 ) ) ;
#1742 = CARTESIAN_POINT ( 'NONE',  ( -12.36094278317000139, 8.718445687105001340, -317.5000000000000000 ) ) ;
#1743 = ORIENTED_EDGE ( 'NONE', *, *, #8760, .T. ) ;
#1744 = AXIS2_PLACEMENT_3D ( 'NONE', #451, #8713, #4585 ) ;
#1745 = CARTESIAN_POINT ( 'NONE',  ( -19.29864983862999850, -3.387441872937999143, -303.6197174156520759 ) ) ;
#1746 = CARTESIAN_POINT ( 'NONE',  ( 18.21319838702001448, -4.476589323548002319, -317.5770954168139610 ) ) ;
#1747 = CARTESIAN_POINT ( 'NONE',  ( -37.87192209818999800, -2.500000000000000000, -461.0868123482000556 ) ) ;
#1748 = CARTESIAN_POINT ( 'NONE',  ( -1.813125098999968543, -7.427867185880000278, -434.7536662776001322 ) ) ;
#1749 = CARTESIAN_POINT ( 'NONE',  ( -34.39269738225353024, -7.500000000000000000, -407.7262955260336525 ) ) ;
#1750 = ORIENTED_EDGE ( 'NONE', *, *, #3580, .F. ) ;
#1751 = CYLINDRICAL_SURFACE ( 'NONE', #1457, 3.499999999999997335 ) ;
#1752 = EDGE_CURVE ( 'NONE', #1322, #1779, #6013, .T. ) ;
#1753 = FACE_OUTER_BOUND ( 'NONE', #3988, .T. ) ;
#1754 = ORIENTED_EDGE ( 'NONE', *, *, #3459, .T. ) ;
#1755 = CIRCLE ( 'NONE', #3123, 3.500000000000003997 ) ;
#1756 = CARTESIAN_POINT ( 'NONE',  ( -17.08426003144000305, -6.624354047749995367, 190.4207385301700128 ) ) ;
#1757 = CARTESIAN_POINT ( 'NONE',  ( -34.39269738225353024, -2.500000000000000000, -407.7262955260336525 ) ) ;
#1758 = DIRECTION ( 'NONE',  ( 0.000000000000000000, -1.000000000000000000, 0.000000000000000000 ) ) ;
#1759 = EDGE_CURVE ( 'NONE', #6366, #4799, #1002, .T. ) ;
#1760 = LINE ( 'NONE', #9929, #4624 ) ;
#1761 = CARTESIAN_POINT ( 'NONE',  ( -6.403271823880001712, 11.84773780780999530, 191.1197171614399792 ) ) ;
#1762 = CARTESIAN_POINT ( 'NONE',  ( 16.99702983282000091, -1.298346578676000007, 314.8616023057000461 ) ) ;
#1763 =( LENGTH_UNIT ( ) NAMED_UNIT ( * ) SI_UNIT ( .MILLI., .METRE. ) );
#1764 = LINE ( 'NONE', #5952, #10510 ) ;
#1765 = VECTOR ( 'NONE', #5247, 1000.000000000000000 ) ;
#1766 = CARTESIAN_POINT ( 'NONE',  ( -17.87038977196999312, -4.940238929760003117, 320.0770942683900557 ) ) ;
#1767 = DIRECTION ( 'NONE',  ( 0.6276613564376926080, 0.000000000000000000, -0.7784864941890744516 ) ) ;
#1768 = CARTESIAN_POINT ( 'NONE',  ( -17.74743742734689178, 5.798256014711220097, -303.5000000000000000 ) ) ;
#1769 = CARTESIAN_POINT ( 'NONE',  ( 17.34710322845000263, -0.4172063223308000168, 314.6383426456000052 ) ) ;
#1770 = ORIENTED_EDGE ( 'NONE', *, *, #4366, .T. ) ;
#1771 = CARTESIAN_POINT ( 'NONE',  ( -9.974269275089660880, -10.84391064191636644, 190.9999999999995737 ) ) ;
#1772 = CARTESIAN_POINT ( 'NONE',  ( -12.02088824526999211, 10.08549396686999522, 319.5792614743400009 ) ) ;
#1773 = ORIENTED_EDGE ( 'NONE', *, *, #3982, .F. ) ;
#1774 = EDGE_CURVE ( 'NONE', #9600, #5739, #2422, .T. ) ;
#1775 = FACE_OUTER_BOUND ( 'NONE', #748, .T. ) ;
#1776 = CARTESIAN_POINT ( 'NONE',  ( -11.33727843270404634, 7.061073773682574384, 315.0000000000000000 ) ) ;
#1777 = ITEM_DEFINED_TRANSFORMATION ( 'NONE', 'NONE', #1476,  #2817 ) ;
#1778 = CARTESIAN_POINT ( 'NONE',  ( -15.00000000000000000, 0.000000000000000000, -285.0000000000000000 ) ) ;
#1779 = VERTEX_POINT ( 'NONE', #5592 ) ;
#1780 = CARTESIAN_POINT ( 'NONE',  ( -0.6695406252879771980, -2.501212138556309306, -434.1886289273209627 ) ) ;
#1781 = CARTESIAN_POINT ( 'NONE',  ( -50.43337757792475173, -2.500000000000000000, -464.9351226150769207 ) ) ;
#1782 = AXIS2_PLACEMENT_3D ( 'NONE', #9436, #9485, #2981 ) ;
#1783 = CARTESIAN_POINT ( 'NONE',  ( 9.616122863433998802, 9.909251266138999981, 190.0000000000000000 ) ) ;
#1784 = LINE ( 'NONE', #9206, #10450 ) ;
#1785 = CARTESIAN_POINT ( 'NONE',  ( -0.1791381520249625270, -2.339610688496001512, -433.8702690752436411 ) ) ;
#1786 = LINE ( 'NONE', #5056, #7970 ) ;
#1787 = CARTESIAN_POINT ( 'NONE',  ( 1.601785992426999705, 12.47016740323998718, -316.3802825947000201 ) ) ;
#1788 = TOROIDAL_SURFACE ( 'NONE', #9510, 15.50000000000000000, 0.5000000000000000000 ) ;
#1789 = FACE_OUTER_BOUND ( 'NONE', #8669, .T. ) ;
#1790 = CARTESIAN_POINT ( 'NONE',  ( -1.009071087474297190, -7.440846336948001571, -435.0353261705186583 ) ) ;
#1791 = DIRECTION ( 'NONE',  ( 0.000000000000000000, -1.000000000000000000, 0.000000000000000000 ) ) ;
#1792 = CARTESIAN_POINT ( 'NONE',  ( 15.47196055635296119, -3.911380178888624215, -315.0000000000000568 ) ) ;
#1793 = ORIENTED_EDGE ( 'NONE', *, *, #9309, .F. ) ;
#1794 = CARTESIAN_POINT ( 'NONE',  ( 7.237892782308166240, -9.087442202657101120, -314.5335583295243964 ) ) ;
#1795 = AXIS2_PLACEMENT_3D ( 'NONE', #9777, #7308, #1558 ) ;
#1796 = ORIENTED_EDGE ( 'NONE', *, *, #9999, .T. ) ;
#1797 = CARTESIAN_POINT ( 'NONE',  ( 4.878402812341999351, 11.12254092566999830, -317.5000000000000000 ) ) ;
#1798 = ORIENTED_EDGE ( 'NONE', *, *, #867, .F. ) ;
#1799 = CIRCLE ( 'NONE', #4031, 14.00000000000000888 ) ;
#1800 = CARTESIAN_POINT ( 'NONE',  ( 16.88084019735002173, -6.719348373024005561, -303.6197174156509391 ) ) ;
#1801 = ADVANCED_FACE ( 'NONE', ( #8069 ), #1517, .F. ) ;
#1802 = CARTESIAN_POINT ( 'NONE',  ( 15.69339834701000136, -7.228928788388996551, -317.5770954168139610 ) ) ;
#1803 = DIRECTION ( 'NONE',  ( -0.000000000000000000, 1.000000000000000000, 0.000000000000000000 ) ) ;
#1804 = AXIS2_PLACEMENT_3D ( 'NONE', #6758, #9066, #9923 ) ;
#1805 = DIRECTION ( 'NONE',  ( 1.000000000000000000, 0.000000000000000000, 0.000000000000000000 ) ) ;
#1806 = SHAPE_REPRESENTATION ( 'Handle', ( #2817 ), #8168 ) ;
#1807 = EDGE_CURVE ( 'NONE', #6443, #6958, #3284, .T. ) ;
#1808 = CARTESIAN_POINT ( 'NONE',  ( 17.70828763765000247, 5.833668797872996414, -303.6197174156520759 ) ) ;
#1809 = CARTESIAN_POINT ( 'NONE',  ( -2.000000000000000000, 3.500000000000000000, -404.4999999999999432 ) ) ;
#1810 = ORIENTED_EDGE ( 'NONE', *, *, #5332, .T. ) ;
#1811 = CARTESIAN_POINT ( 'NONE',  ( -16.58659719219999928, -2.947707964209000053, -314.6383426456000052 ) ) ;
#1812 = ADVANCED_FACE ( 'NONE', ( #5643 ), #8755, .T. ) ;
#1813 = CARTESIAN_POINT ( 'NONE',  ( 2.001531325394999783, 11.45199047667999892, -302.5000000000000000 ) ) ;
#1814 = ORIENTED_EDGE ( 'NONE', *, *, #6930, .T. ) ;
#1815 = CARTESIAN_POINT ( 'NONE',  ( 11.20196042648000123, -10.44833032063000111, 190.4207385301700128 ) ) ;
#1816 = CARTESIAN_POINT ( 'NONE',  ( 17.19853431801041665, -2.231396706186351775, -315.0000000000001137 ) ) ;
#1817 = FACE_OUTER_BOUND ( 'NONE', #10400, .T. ) ;
#1818 = DIRECTION ( 'NONE',  ( -0.8820010751365675583, 0.000000000000000000, -0.4712473909295825103 ) ) ;
#1819 = CARTESIAN_POINT ( 'NONE',  ( 19.86706274963002983, 1.898735342979001484, 190.4207385301700128 ) ) ;
#1820 = CARTESIAN_POINT ( 'NONE',  ( 17.14577796628000073, -0.02050488658304000164, 314.8616023057000461 ) ) ;
#1821 =( NAMED_UNIT ( * ) PLANE_ANGLE_UNIT ( ) SI_UNIT ( $, .RADIAN. ) );
#1822 = CARTESIAN_POINT ( 'NONE',  ( -119.6503683519543983, -2.500000000000000000, -299.0840866897705155 ) ) ;
#1823 = CARTESIAN_POINT ( 'NONE',  ( -19.59064078059999758, -0.07061976926606000626, 320.0770942683900557 ) ) ;
#1824 = DIRECTION ( 'NONE',  ( 0.000000000000000000, 1.000000000000000000, -0.000000000000000000 ) ) ;
#1825 = LINE ( 'NONE', #5841, #9195 ) ;
#1826 = CARTESIAN_POINT ( 'NONE',  ( 16.77099092997999819, 1.279831385791999843, 315.0848619657999734 ) ) ;
#1827 = EDGE_LOOP ( 'NONE', ( #5391, #2707, #3495, #4698 ) ) ;
#1828 = CARTESIAN_POINT ( 'NONE',  ( -2.000000000000000000, -10.50000000000000000, -414.5000000000000000 ) ) ;
#1829 = ORIENTED_EDGE ( 'NONE', *, *, #9368, .T. ) ;
#1830 = CARTESIAN_POINT ( 'NONE',  ( -7.514439085588995759, 11.67576679883001667, 319.5792614743400009 ) ) ;
#1831 = CARTESIAN_POINT ( 'NONE',  ( -15.00000000000000000, 0.000000000000000000, -285.0000000000000000 ) ) ;
#1832 = SHAPE_REPRESENTATION ( 'Counter Blade', ( #2817 ), #5369 ) ;
#1833 = LINE ( 'NONE', #856, #311 ) ;
#1834 = CARTESIAN_POINT ( 'NONE',  ( 7.042505780985288233, 8.656073623659681360, 315.0000000000000000 ) ) ;
#1835 = CARTESIAN_POINT ( 'NONE',  ( -37.82921798586427542, -9.000000000000001776, -422.3602549205905916 ) ) ;
#1836 = ORIENTED_EDGE ( 'NONE', *, *, #7471, .T. ) ;
#1837 = CARTESIAN_POINT ( 'NONE',  ( 16.15280651819000113, -6.039793344733999980, -302.5000000000000000 ) ) ;
#1838 = CARTESIAN_POINT ( 'NONE',  ( 7.347903365571999856, 10.60600056872999986, 190.0000000000000000 ) ) ;
#1839 = CARTESIAN_POINT ( 'NONE',  ( 17.05540563375874541, -2.295823697340080738, 314.4999398562650867 ) ) ;
#1840 = CARTESIAN_POINT ( 'NONE',  ( -15.00000000000072120, 0.4945770392355430256, -284.9999999999999432 ) ) ;
#1841 = FACE_BOUND ( 'NONE', #5066, .T. ) ;
#1842 = CARTESIAN_POINT ( 'NONE',  ( 9.378959784071181360, -4.100000000000000533, -525.1866552614185366 ) ) ;
#1843 = CARTESIAN_POINT ( 'NONE',  ( 7.441755802380456863, -5.633964924930761065, -525.6644890118283229 ) ) ;
#1844 = UNCERTAINTY_MEASURE_WITH_UNIT (LENGTH_MEASURE( 1.000000000000000082E-05 ), #3000, 'distance_accuracy_value', 'NONE');
#1845 = CARTESIAN_POINT ( 'NONE',  ( 15.67978886374999803, 4.575336738469999887, -315.0000000000000000 ) ) ;
#1846 = CARTESIAN_POINT ( 'NONE',  ( 16.03969916442340704, -3.142024325209859636, -315.0000000000000568 ) ) ;
#1847 = ORIENTED_EDGE ( 'NONE', *, *, #7977, .F. ) ;
#1848 = CIRCLE ( 'NONE', #2708, 1.000000000000008882 ) ;
#1849 = CARTESIAN_POINT ( 'NONE',  ( 15.67978886374999803, 4.575336738469999887, -315.0000000000001137 ) ) ;
#1850 = CARTESIAN_POINT ( 'NONE',  ( -19.99999036626000048, -4.642009783819999925E-09, -316.5000000000000000 ) ) ;
#1851 = ORIENTED_EDGE ( 'NONE', *, *, #10227, .T. ) ;
#1852 = CARTESIAN_POINT ( 'NONE',  ( 18.32252861763999974, 3.123808493131999597, -317.4999999999870397 ) ) ;
#1853 = ORIENTED_EDGE ( 'NONE', *, *, #2590, .F. ) ;
#1854 = CARTESIAN_POINT ( 'NONE',  ( 17.60469080286000931, 4.126100741655001514, -317.4928077629770087 ) ) ;
#1855 = CARTESIAN_POINT ( 'NONE',  ( -18.86307259346999032, 0.4762574081846996932, -317.4928077629770087 ) ) ;
#1856 = MANIFOLD_SOLID_BREP ( 'Stock-MAS-686-1', #5554 ) ;
#1857 = FACE_OUTER_BOUND ( 'NONE', #1966, .T. ) ;
#1858 = AXIS2_PLACEMENT_3D ( 'NONE', #7847, #8650, #4626 ) ;
#1859 = CARTESIAN_POINT ( 'NONE',  ( -9.252434838928003558, 11.08696499602999630, -303.6197174156509391 ) ) ;
#1860 = CARTESIAN_POINT ( 'NONE',  ( 10.32803372116435270, 10.00000000000000178, 315.0000000000000000 ) ) ;
#1861 = ORIENTED_EDGE ( 'NONE', *, *, #7909, .T. ) ;
#1862 = DIRECTION ( 'NONE',  ( 0.000000000000000000, -1.000000000000000000, 0.000000000000000000 ) ) ;
#1863 = CARTESIAN_POINT ( 'NONE',  ( 0.1867348994714999877, 11.51775814840000045, -302.5000000000000000 ) ) ;
#1864 = VERTEX_POINT ( 'NONE', #7267 ) ;
#1865 = CARTESIAN_POINT ( 'NONE',  ( 3.136708848033998187, -12.44064353863999983, 190.4207385301700128 ) ) ;
#1866 = CARTESIAN_POINT ( 'NONE',  ( -15.67978886374999803, -4.575336738469999887, -315.0000000000001137 ) ) ;
#1867 = CARTESIAN_POINT ( 'NONE',  ( 11.74249363970098514, 6.849480045866885192, -315.0000000000000000 ) ) ;
#1868 = CARTESIAN_POINT ( 'NONE',  ( 12.07524870805000639, 10.05998438363999981, 190.4207385301700128 ) ) ;
#1869 = EDGE_CURVE ( 'NONE', #932, #4003, #7480, .T. ) ;
#1870 = EDGE_LOOP ( 'NONE', ( #10144, #6393 ) ) ;
#1871 = CARTESIAN_POINT ( 'NONE',  ( 11.96281778373999849, -6.662668310474999522, 315.0848619657999734 ) ) ;
#1872 = DIRECTION ( 'NONE',  ( 0.000000000000000000, 1.000000000000000000, 0.000000000000000000 ) ) ;
#1873 = CARTESIAN_POINT ( 'NONE',  ( -12.03361782604000219, -9.527744202155000508, 320.0770942683900557 ) ) ;
#1874 = DIRECTION ( 'NONE',  ( 0.000000000000000000, 1.000000000000000000, -0.000000000000000000 ) ) ;
#1875 = CARTESIAN_POINT ( 'NONE',  ( -11.72170966038013340, 10.14138702413947968, -303.4999999999990905 ) ) ;
#1876 = CARTESIAN_POINT ( 'NONE',  ( 3.846123575835999731, 9.203727088275000412, 315.0848619657999734 ) ) ;
#1877 = ORIENTED_EDGE ( 'NONE', *, *, #4570, .F. ) ;
#1878 = CARTESIAN_POINT ( 'NONE',  ( 13.99679147458261141, -8.939383429014133853, 190.9999999999995737 ) ) ;
#1879 = CARTESIAN_POINT ( 'NONE',  ( 11.25912153621000300, 10.42419777155999938, 319.5792614743400009 ) ) ;
#1880 = EDGE_CURVE ( 'NONE', #10437, #4923, #3628, .T. ) ;
#1881 = EDGE_CURVE ( 'NONE', #1689, #1519, #4653, .T. ) ;
#1882 = CARTESIAN_POINT ( 'NONE',  ( -12.67186291068377102, -4.210876960398400648, -439.0233713709748145 ) ) ;
#1883 = CARTESIAN_POINT ( 'NONE',  ( 4.669690493011572130, 9.131031402067035785, 315.0000000000001137 ) ) ;
#1884 = CARTESIAN_POINT ( 'NONE',  ( 14.79012398733999945, -1.483731117707000058, -285.0000000000000000 ) ) ;
#1885 = ORIENTED_EDGE ( 'NONE', *, *, #3973, .T. ) ;
#1886 = CIRCLE ( 'NONE', #4802, 1.000010080120980804 ) ;
#1887 = CARTESIAN_POINT ( 'NONE',  ( 11.28854116844999922, -9.238965579841000419, -302.5000000000000000 ) ) ;
#1888 = VECTOR ( 'NONE', #9928, 1000.000000000000000 ) ;
#1889 = SURFACE_SIDE_STYLE ('',( #10003 ) ) ;
#1890 = CARTESIAN_POINT ( 'NONE',  ( 17.81342281586000098, 3.988456401492999959, 190.0000000000000000 ) ) ;
#1891 = EDGE_CURVE ( 'NONE', #1322, #2247, #9793, .T. ) ;
#1892 = CARTESIAN_POINT ( 'NONE',  ( -15.75853520210212011, 3.543431633405213610, -314.9999999999999432 ) ) ;
#1893 = CARTESIAN_POINT ( 'NONE',  ( -18.87263095182001749, -0.3456903499861000983, 190.0071920248299477 ) ) ;
#1894 = DIRECTION ( 'NONE',  ( 0.1247904863035870365, 0.000000000000000000, -0.9921831154218027082 ) ) ;
#1895 = AXIS2_PLACEMENT_3D ( 'NONE', #7059, #1402, #2107 ) ;
#1896 = CARTESIAN_POINT ( 'NONE',  ( 6.760923308610696125, -4.443194654328453730, -525.3178833974152440 ) ) ;
#1897 = FACE_OUTER_BOUND ( 'NONE', #2231, .T. ) ;
#1898 = CARTESIAN_POINT ( 'NONE',  ( -12.86189863199293093, -5.758762107780500017, -438.9337381413729418 ) ) ;
#1899 = ORIENTED_EDGE ( 'NONE', *, *, #7170, .T. ) ;
#1900 = CARTESIAN_POINT ( 'NONE',  ( 7.560581757588001217, 10.42594579828999990, 319.9928079742500131 ) ) ;
#1901 = AXIS2_PLACEMENT_3D ( 'NONE', #2432, #3345, #5855 ) ;
#1902 = CARTESIAN_POINT ( 'NONE',  ( 14.97237716209997416, -8.305886502593784471, -316.5000000000004547 ) ) ;
#1903 = ORIENTED_EDGE ( 'NONE', *, *, #444, .T. ) ;
#1904 = DIRECTION ( 'NONE',  ( -0.5828070674935416084, 0.000000000000000000, -0.8126105599114364919 ) ) ;
#1905 = ORIENTED_EDGE ( 'NONE', *, *, #4115, .F. ) ;
#1906 = CIRCLE ( 'NONE', #4643, 0.5000000000000004441 ) ;
#1907 = DIRECTION ( 'NONE',  ( 0.000000000000000000, -1.000000000000000000, 0.000000000000000000 ) ) ;
#1908 = CARTESIAN_POINT ( 'NONE',  ( 19.60211473220001110, -0.3233313581039002904, -317.5770954168139610 ) ) ;
#1909 = EDGE_CURVE ( 'NONE', #1864, #4012, #8125, .T. ) ;
#1910 = PLANE ( 'NONE',  #9008 ) ;
#1911 = LINE ( 'NONE', #5984, #3303 ) ;
#1912 = CARTESIAN_POINT ( 'NONE',  ( -11.54127207300577496, -7.525448855209205590, 314.4999468205385256 ) ) ;
#1913 = ORIENTED_EDGE ( 'NONE', *, *, #233, .T. ) ;
#1914 = CARTESIAN_POINT ( 'NONE',  ( 13.46369163363000077, -8.092480683229998917, 190.0000000000000000 ) ) ;
#1915 = DIRECTION ( 'NONE',  ( 0.000000000000000000, -1.000000000000000000, 0.000000000000000000 ) ) ;
#1916 = ORIENTED_EDGE ( 'NONE', *, *, #4947, .T. ) ;
#1917 = FACE_OUTER_BOUND ( 'NONE', #7814, .T. ) ;
#1918 = LINE ( 'NONE', #1054, #6408 ) ;
#1919 = DIRECTION ( 'NONE',  ( 0.000000000000000000, 1.000000000000000000, -0.000000000000000000 ) ) ;
#1920 = CARTESIAN_POINT ( 'NONE',  ( 13.97596040350999402, 9.042973024665997173, 190.4207385301700128 ) ) ;
#1921 = ADVANCED_FACE ( 'NONE', ( #4094 ), #2768, .T. ) ;
#1922 = DIRECTION ( 'NONE',  ( 0.9921831154218023752, -0.000000000000000000, 0.1247904863035890627 ) ) ;
#1923 = CARTESIAN_POINT ( 'NONE',  ( 1.279515965483999906E-07, 10.00000000755999885, 190.0000000000000000 ) ) ;
#1924 = PRODUCT ( 'Lower Jaw Base Arm', 'Lower Jaw Base Arm', '', ( #5587 ) ) ;
#1925 = CARTESIAN_POINT ( 'NONE',  ( 17.67524584885999772, -5.985122643678997711, 319.5792614743400009 ) ) ;
#1926 = VECTOR ( 'NONE', #8462, 1000.000000000000000 ) ;
#1927 = LINE ( 'NONE', #7567, #7093 ) ;
#1928 = CARTESIAN_POINT ( 'NONE',  ( 14.72449281369000040, -5.549439731021000632, -314.4150829855000211 ) ) ;
#1929 = CARTESIAN_POINT ( 'NONE',  ( 17.42228208267999889, 1.444224815522999972, 314.4150829855000211 ) ) ;
#1930 = ORIENTED_EDGE ( 'NONE', *, *, #3836, .T. ) ;
#1931 = CARTESIAN_POINT ( 'NONE',  ( 19.99999721801999897, 7.771189452710000131E-11, 191.0000000000000000 ) ) ;
#1932 = CARTESIAN_POINT ( 'NONE',  ( -20.05691607070997051, -0.5615793767616999999, 319.5792614743400009 ) ) ;
#1933 = EDGE_CURVE ( 'NONE', #7812, #7526, #9428, .T. ) ;
#1934 = VECTOR ( 'NONE', #3840, 1000.000000000000000 ) ;
#1935 = AXIS2_PLACEMENT_3D ( 'NONE', #2781, #10140, #6053 ) ;
#1936 = CARTESIAN_POINT ( 'NONE',  ( -13.08309215884270138, -3.120241701627000985, -437.9645355315274173 ) ) ;
#1937 = CARTESIAN_POINT ( 'NONE',  ( -9.217211940708146756, 7.977736869146946574, 315.0000000000000000 ) ) ;
#1938 = CARTESIAN_POINT ( 'NONE',  ( 14.79012398734008293, -1.483731117706880154, -284.9999999999999432 ) ) ;
#1939 = CARTESIAN_POINT ( 'NONE',  ( 17.63021146919999893, -4.299866645372000029, -302.4999999999969873 ) ) ;
#1940 = EDGE_CURVE ( 'NONE', #223, #8573, #5502, .T. ) ;
#1941 =( NAMED_UNIT ( * ) PLANE_ANGLE_UNIT ( ) SI_UNIT ( $, .RADIAN. ) );
#1942 = DIRECTION ( 'NONE',  ( -0.8126105599114364919, 6.772514207610136972E-17, 0.5828070674935419415 ) ) ;
#1943 = ADVANCED_FACE ( 'NONE', ( #2115 ), #6140, .F. ) ;
#1944 = CARTESIAN_POINT ( 'NONE',  ( -16.37160231057345783, 2.539265572400264848, -315.0000000000001137 ) ) ;
#1945 = AXIS2_PLACEMENT_3D ( 'NONE', #7118, #3996, #10385 ) ;
#1946 = CARTESIAN_POINT ( 'NONE',  ( 5.118368704603114087E-10, 10.00000000003099210, 314.4999681336588537 ) ) ;
#1947 = CARTESIAN_POINT ( 'NONE',  ( -1.813125407131493949, -2.572135581867000198, -434.7536649739391237 ) ) ;
#1948 = FACE_BOUND ( 'NONE', #10054, .T. ) ;
#1949 = CARTESIAN_POINT ( 'NONE',  ( 7.681427628432651922, -5.663384406618502176, -525.7189183918870867 ) ) ;
#1950 = UNCERTAINTY_MEASURE_WITH_UNIT (LENGTH_MEASURE( 1.000000000000000082E-05 ), #10396, 'distance_accuracy_value', 'NONE');
#1951 = CYLINDRICAL_SURFACE ( 'NONE', #8230, 5.000000000000004441 ) ;
#1952 = EDGE_CURVE ( 'NONE', #8193, #5743, #2223, .T. ) ;
#1953 = VERTEX_POINT ( 'NONE', #7117 ) ;
#1954 = CARTESIAN_POINT ( 'NONE',  ( 6.240232637630001911, 10.74449313720999832, 319.9928079742500131 ) ) ;
#1955 = CARTESIAN_POINT ( 'NONE',  ( -1.602145841528213932, -12.47735433440135644, -316.5000000000004547 ) ) ;
#1956 = PLANE ( 'NONE',  #2955 ) ;
#1957 = ORIENTED_EDGE ( 'NONE', *, *, #4434, .F. ) ;
#1958 = DIRECTION ( 'NONE',  ( -0.9902680687415801319, 0.000000000000000000, -0.1391731009599957991 ) ) ;
#1959 = CARTESIAN_POINT ( 'NONE',  ( -18.19038122738000141, -4.511441183124001775, -317.5770954168139610 ) ) ;
#1960 = AXIS2_PLACEMENT_3D ( 'NONE', #9757, #2288, #832 ) ;
#1961 = CARTESIAN_POINT ( 'NONE',  ( -15.60185585328000002, 4.689707898928999974, -314.4150829855000211 ) ) ;
#1962 = VERTEX_POINT ( 'NONE', #1306 ) ;
#1963 = AXIS2_PLACEMENT_3D ( 'NONE', #9374, #4374, #10069 ) ;
#1964 = CARTESIAN_POINT ( 'NONE',  ( 7.251913689787688355, 9.130298775770077313, -314.5336966332660040 ) ) ;
#1965 = AXIS2_PLACEMENT_3D ( 'NONE', #2797, #6170, #4507 ) ;
#1966 = EDGE_LOOP ( 'NONE', ( #6027, #7387 ) ) ;
#1967 = CARTESIAN_POINT ( 'NONE',  ( -38.33299437316763658, -7.500000000000000000, -461.6435047520546391 ) ) ;
#1968 = CYLINDRICAL_SURFACE ( 'NONE', #9194, 0.7499999999999997780 ) ;
#1969 = EDGE_LOOP ( 'NONE', ( #10293, #852, #7468, #7336, #5645 ) ) ;
#1970 = CARTESIAN_POINT ( 'NONE',  ( -18.20422786544000715, -5.185156308378004120, 191.1197171614399792 ) ) ;
#1971 = ORIENTED_EDGE ( 'NONE', *, *, #10530, .T. ) ;
#1972 = FACE_BOUND ( 'NONE', #4751, .T. ) ;
#1973 = DIRECTION ( 'NONE',  ( 0.000000000000000000, -1.000000000000000000, 0.000000000000000000 ) ) ;
#1974 = LINE ( 'NONE', #1262, #10038 ) ;
#1975 = CIRCLE ( 'NONE', #4723, 15.50000000000001421 ) ;
#1976 = CIRCLE ( 'NONE', #6248, 3.500000000000003109 ) ;
#1977 = CARTESIAN_POINT ( 'NONE',  ( -0.5023555725018206131, -7.489090630217000388, -434.1119911457818716 ) ) ;
#1978 = SURFACE_SIDE_STYLE ('',( #6922 ) ) ;
#1979 = LINE ( 'NONE', #6154, #1765 ) ;
#1980 = CARTESIAN_POINT ( 'NONE',  ( -14.92426358056000701, -8.426786174986000688, 319.5792614743400009 ) ) ;
#1981 = B_SPLINE_CURVE_WITH_KNOTS ( 'NONE', 3,
 ( #2403, #5671, #2186, #4660, #3856, #7186, #1601, #8955, #4874, #10455, #6313, #5509, #3096, #1050, #1649, #5725, #3370, #8411, #1813, #1863, #8358, #2560, #5828, #3476, #3531, #4284, #2674, #9816, #145, #996, #2456, #4334, #7607, #9173, #6698, #9976, #2617, #7556, #201 ),
 .UNSPECIFIED., .F., .F.,
 ( 4, 1, 1, 1, 1, 1, 1, 1, 1, 1, 1, 1, 1, 1, 1, 1, 1, 1, 1, 1, 1, 1, 1, 1, 1, 1, 1, 1, 1, 1, 1, 1, 1, 1, 1, 1, 4 ),
 ( 0.000000000000000000, 0.02777777777778000015, 0.05555555555556000030, 0.08333333333333001192, 0.1111111111111000027, 0.1388888888888999973, 0.1666666666667000196, 0.1944444444444000109, 0.2222222222222000054, 0.2500000000000000000, 0.2777777777777999946, 0.3055555555555999891, 0.3333333333333000081, 0.3611111111111000027, 0.3888888888888999973, 0.4166666666666999919, 0.4444444444444000109, 0.4722222222222000054, 0.5000000000000000000, 0.5277777777777999946, 0.5555555555555999891, 0.5833333333333000637, 0.6111111111111000582, 0.6388888888888999418, 0.6666666666667000474, 0.6944444444444000109, 0.7222222222222000054, 0.7500000000000000000, 0.7777777777777999946, 0.8055555555555999891, 0.8333333333333000637, 0.8611111111111000582, 0.8888888888888999418, 0.9166666666667000474, 0.9444444444444000109, 0.9722222222222000054, 1.000000000000000000 ),
 .UNSPECIFIED. ) ;
#1982 = CARTESIAN_POINT ( 'NONE',  ( 14.00000000000000000, -2.500000000000000000, -417.5000000000000000 ) ) ;
#1983 = CARTESIAN_POINT ( 'NONE',  ( -16.60805916514000202, 2.908391789136000050, 314.6383426456000052 ) ) ;
#1984 = VERTEX_POINT ( 'NONE', #5436 ) ;
#1985 = LINE ( 'NONE', #2188, #10502 ) ;
#1986 = ORIENTED_EDGE ( 'NONE', *, *, #3319, .T. ) ;
#1987 = CARTESIAN_POINT ( 'NONE',  ( -0.6780083913994491285, -7.498182470000450017, -434.1985855385974560 ) ) ;
#1988 = PRESENTATION_LAYER_ASSIGNMENT (  '', '', ( #3362 ) ) ;
#1989 = CARTESIAN_POINT ( 'NONE',  ( -1.624818744522249503, -7.500000000000000888, -412.9798331893018712 ) ) ;
#1990 = CARTESIAN_POINT ( 'NONE',  ( -47.11589368967775471, -7.500000000000000888, -410.8439258096980780 ) ) ;
#1991 = CARTESIAN_POINT ( 'NONE',  ( 7.006889269069000115, -6.844138725329000472, 315.0000000000001705 ) ) ;
#1992 = COLOUR_RGB ( '', 0.31764706, 0.68627451, 0.89019608) ;
#1993 = DIRECTION ( 'NONE',  ( 0.000000000000000000, -1.000000000000000000, 0.000000000000000000 ) ) ;
#1994 = SURFACE_STYLE_USAGE ( .BOTH. , #6281 ) ;
#1995 = EDGE_CURVE ( 'NONE', #1689, #8136, #1197, .T. ) ;
#1996 = CARTESIAN_POINT ( 'NONE',  ( 1.514429654104534930E-09, 10.00000000000000000, -302.5000000000000000 ) ) ;
#1997 = CARTESIAN_POINT ( 'NONE',  ( 9.526067998327799539E-10, -10.00000000005854339, 314.4999528359535361 ) ) ;
#1998 = CARTESIAN_POINT ( 'NONE',  ( 7.284698641071005731, 10.49877923466000063, 190.0071920248299477 ) ) ;
#1999 = DIRECTION ( 'NONE',  ( 0.000000000000000000, -1.000000000000000000, -0.000000000000000000 ) ) ;
#2000 = STYLED_ITEM ( 'NONE', ( #6479 ), #453 ) ;
#2001 = CARTESIAN_POINT ( 'NONE',  ( -18.86945318303000008, -1.615078380336999908, -317.5000000000470095 ) ) ;
#2002 = EDGE_CURVE ( 'NONE', #5421, #3371, #10333, .T. ) ;
#2003 = CARTESIAN_POINT ( 'NONE',  ( 8.342417508530179049, -5.749081105070941611, -525.7122382318706286 ) ) ;
#2004 = CARTESIAN_POINT ( 'NONE',  ( 10.90962076852776796, -7.272180451173178461, 315.0000000000000000 ) ) ;
#2005 = CARTESIAN_POINT ( 'NONE',  ( 3.874983216044999956, 9.425407904674999671, -314.8616023057000461 ) ) ;
#2006 = ORIENTED_EDGE ( 'NONE', *, *, #3523, .T. ) ;
#2007 = CARTESIAN_POINT ( 'NONE',  ( -2.482300462934001306, 11.29873291818999803, 319.9928079742500131 ) ) ;
#2008 = CARTESIAN_POINT ( 'NONE',  ( 2.055855549839187280, -12.45069410617974626, -316.5000000000004547 ) ) ;
#2009 = DIRECTION ( 'NONE',  ( 0.2381566831044910626, 0.000000000000000000, -0.9712267471052612455 ) ) ;
#2010 = VERTEX_POINT ( 'NONE', #4526 ) ;
#2011 = CARTESIAN_POINT ( 'NONE',  ( -11.29610983636999144, 9.103527074753996473, -317.4928077629770087 ) ) ;
#2012 = CARTESIAN_POINT ( 'NONE',  ( 20.10152810630999554, -0.3450717431897997733, -317.0792622552969533 ) ) ;
#2013 = EDGE_CURVE ( 'NONE', #9376, #2675, #372, .T. ) ;
#2014 = CARTESIAN_POINT ( 'NONE',  ( -16.97404422732000029, 2.118410180888999683, -314.6383426456000052 ) ) ;
#2015 = DIRECTION ( 'NONE',  ( 1.000000000000000000, 0.000000000000000000, 0.000000000000000000 ) ) ;
#2016 = ORIENTED_EDGE ( 'NONE', *, *, #4776, .F. ) ;
#2017 = CARTESIAN_POINT ( 'NONE',  ( -5.950428891765999317, -10.92854977363000124, 190.0000000000000000 ) ) ;
#2018 = CARTESIAN_POINT ( 'NONE',  ( -72.90663470102438737, 7.399494936611693774, -368.2168990826883146 ) ) ;
#2019 = ORIENTED_EDGE ( 'NONE', *, *, #4921, .T. ) ;
#2020 = CARTESIAN_POINT ( 'NONE',  ( -16.34352199340000311, -7.209047878930006092, 191.1197171614399792 ) ) ;
#2021 = ORIENTED_EDGE ( 'NONE', *, *, #4165, .F. ) ;
#2022 = CARTESIAN_POINT ( 'NONE',  ( -46.74071243419621169, -9.500000000000001776, -414.3237589990241077 ) ) ;
#2023 = CARTESIAN_POINT ( 'NONE',  ( -8.965618380443995505, -10.00899073891999436, -302.5071922382879279 ) ) ;
#2024 = EDGE_CURVE ( 'NONE', #22, #8305, #5870, .T. ) ;
#2025 = CARTESIAN_POINT ( 'NONE',  ( -1.873948611767810357, -7.500000000000000000, -349.2478646809746579 ) ) ;
#2026 = CIRCLE ( 'NONE', #9059, 15.00000000000000533 ) ;
#2027 = CARTESIAN_POINT ( 'NONE',  ( -0.5174164570134516250, -7.488494838810996868, -434.0682185966899169 ) ) ;
#2028 = CARTESIAN_POINT ( 'NONE',  ( 5.068019528653000982, 10.96907295785000080, -302.5071922382879279 ) ) ;
#2029 = CARTESIAN_POINT ( 'NONE',  ( -19.50549492440999089, -2.789745814424999359, 318.8802828394900644 ) ) ;
#2030 = CARTESIAN_POINT ( 'NONE',  ( 16.90798586812000082, 0.2930809059028999797, -315.0848619657999734 ) ) ;
#2031 = CARTESIAN_POINT ( 'NONE',  ( -16.97404422732000029, 2.118410180888999683, 314.6383426456000052 ) ) ;
#2032 = ORIENTED_EDGE ( 'NONE', *, *, #3049, .T. ) ;
#2033 = CARTESIAN_POINT ( 'NONE',  ( -0.6878067384152003472, -11.39249343872000075, 190.0071920248299477 ) ) ;
#2034 = ORIENTED_EDGE ( 'NONE', *, *, #1553, .F. ) ;
#2035 = CARTESIAN_POINT ( 'NONE',  ( -19.95862339310001943, 0.9382979884530006087, 318.8802828394900644 ) ) ;
#2036 = DIRECTION ( 'NONE',  ( -1.000000000000000000, 0.000000000000000000, 0.000000000000000000 ) ) ;
#2037 = ADVANCED_FACE ( 'NONE', ( #2063 ), #7167, .T. ) ;
#2038 = CARTESIAN_POINT ( 'NONE',  ( -17.57772697299999720, 0.3191603157329000462, 314.4150829855000211 ) ) ;
#2039 = CARTESIAN_POINT ( 'NONE',  ( -31.97945899169042505, -7.500000000000000000, -498.3127369250419747 ) ) ;
#2040 = CARTESIAN_POINT ( 'NONE',  ( -10.00000000000000000, -2.500000000000000000, -285.0000000000000000 ) ) ;
#2041 = CARTESIAN_POINT ( 'NONE',  ( -11.72583169940718406, -6.858410958448124539, -315.0000000000000000 ) ) ;
#2042 = FACE_OUTER_BOUND ( 'NONE', #7532, .T. ) ;
#2043 = PRESENTATION_STYLE_ASSIGNMENT (( #1994 ) ) ;
#2044 = FACE_OUTER_BOUND ( 'NONE', #8934, .T. ) ;
#2045 = CARTESIAN_POINT ( 'NONE',  ( -2.545630254023276251, 9.391959925330709780, -315.0000000000000000 ) ) ;
#2046 = CARTESIAN_POINT ( 'NONE',  ( 14.16528011596000169, 7.496216825914998161, 190.0071920248299477 ) ) ;
#2047 = CARTESIAN_POINT ( 'NONE',  ( -13.30825372127758399, -9.500000000000001776, -400.6612558711213410 ) ) ;
#2048 = EDGE_CURVE ( 'NONE', #3465, #199, #5327, .T. ) ;
#2049 = CARTESIAN_POINT ( 'NONE',  ( -2.000000000000000000, 3.500000000000000000, -414.5000000000000000 ) ) ;
#2050 = AXIS2_PLACEMENT_3D ( 'NONE', #9959, #2545, #7644 ) ;
#2051 = CARTESIAN_POINT ( 'NONE',  ( -38.38033378105252780, -7.500000000000000000, -506.9690816445435644 ) ) ;
#2052 =( NAMED_UNIT ( * ) PLANE_ANGLE_UNIT ( ) SI_UNIT ( $, .RADIAN. ) );
#2053 = CARTESIAN_POINT ( 'NONE',  ( 14.65007096172560708, -4.807726778454477490, 314.9999999999998863 ) ) ;
#2054 = CARTESIAN_POINT ( 'NONE',  ( 12.10743226551000085, 7.094093637544000686, -314.6383426456000052 ) ) ;
#2055 = CARTESIAN_POINT ( 'NONE',  ( -8.586595388443328147, -7.500000000000000000, -526.6836397678595176 ) ) ;
#2056 = CARTESIAN_POINT ( 'NONE',  ( -19.30579288353658640, -3.388955136080751718, -316.5000000000004547 ) ) ;
#2057 = LINE ( 'NONE', #6086, #10332 ) ;
#2058 = ORIENTED_EDGE ( 'NONE', *, *, #6274, .F. ) ;
#2059 = CARTESIAN_POINT ( 'NONE',  ( -37.62994892358009480, -8.000000000000000000, -402.7806230189665371 ) ) ;
#2060 = VECTOR ( 'NONE', #9651, 1000.000000000000000 ) ;
#2061 = AXIS2_PLACEMENT_3D ( 'NONE', #6419, #7392, #730 ) ;
#2062 = CARTESIAN_POINT ( 'NONE',  ( -4.911540754813998433, -11.70462039183999892, -317.5770954168139610 ) ) ;
#2063 = FACE_OUTER_BOUND ( 'NONE', #3743, .T. ) ;
#2064 = CIRCLE ( 'NONE', #1035, 3.499999999999997335 ) ;
#2065 = DIRECTION ( 'NONE',  ( 0.000000000000000000, -1.000000000000000000, 0.000000000000000000 ) ) ;
#2066 = ORIENTED_EDGE ( 'NONE', *, *, #10269, .T. ) ;
#2067 = CARTESIAN_POINT ( 'NONE',  ( 16.83327205402999738, -5.309787193942999473, 190.0000000000000000 ) ) ;
#2068 = EDGE_CURVE ( 'NONE', #7519, #2769, #7910, .T. ) ;
#2069 = CARTESIAN_POINT ( 'NONE',  ( -41.35482467236749926, -8.000000000000000000, -366.8119992166443808 ) ) ;
#2070 = ORIENTED_EDGE ( 'NONE', *, *, #6343, .T. ) ;
#2071 = DIRECTION ( 'NONE',  ( 0.6918631112021627061, 0.000000000000000000, -0.7220286942758327164 ) ) ;
#2072 = ORIENTED_EDGE ( 'NONE', *, *, #9179, .F. ) ;
#2073 = CARTESIAN_POINT ( 'NONE',  ( -17.50000000000000000, 0.000000000000000000, -302.5000000000000000 ) ) ;
#2074 = CARTESIAN_POINT ( 'NONE',  ( 6.297776810737998332, -10.73166643879000404, -302.5071922382879279 ) ) ;
#2075 = DIRECTION ( 'NONE',  ( -0.000000000000000000, 1.000000000000000000, 0.000000000000000000 ) ) ;
#2076 = CARTESIAN_POINT ( 'NONE',  ( -0.7865748771364371450, -7.501119061185001158, -434.2245970632208127 ) ) ;
#2077 = FILL_AREA_STYLE ('',( #4544 ) ) ;
#2078 = ADVANCED_FACE ( 'NONE', ( #4696, #6298, #7972, #6962, #615 ), #7067, .T. ) ;
#2079 = LINE ( 'NONE', #9343, #6392 ) ;
#2080 = CARTESIAN_POINT ( 'NONE',  ( 18.75338617474996994, -4.519296150162002590, 319.5792614743400009 ) ) ;
#2081 = CARTESIAN_POINT ( 'NONE',  ( 15.27200851150000105, -4.387263554753999983, -314.8616023057000461 ) ) ;
#2082 = EDGE_CURVE ( 'NONE', #56, #4107, #2972, .T. ) ;
#2083 = CARTESIAN_POINT ( 'NONE',  ( -17.34500932694999875, 0.6070218422356999932, 314.6383426456000052 ) ) ;
#2084 = ORIENTED_EDGE ( 'NONE', *, *, #8293, .F. ) ;
#2085 = DIRECTION ( 'NONE',  ( -0.9554399839384175586, 0.000000000000000000, -0.2951854283188048989 ) ) ;
#2086 = CARTESIAN_POINT ( 'NONE',  ( -19.12221666159999600, 3.679580603257996962, 318.8802828394900644 ) ) ;
#2087 = CARTESIAN_POINT ( 'NONE',  ( -15.34933947562448076, -6.750000000000000000, -437.7418441346085274 ) ) ;
#2088 = VECTOR ( 'NONE', #1664, 1000.000000000000114 ) ;
#2089 = DIRECTION ( 'NONE',  ( -0.4712473909295860630, 0.000000000000000000, 0.8820010751365656709 ) ) ;
#2090 = CARTESIAN_POINT ( 'NONE',  ( 18.95677580539999951, 0.9180370088860999589, 320.0000000000000000 ) ) ;
#2091 = CARTESIAN_POINT ( 'NONE',  ( 13.57573464316000056, -3.225916527208000151, -284.9999999999999432 ) ) ;
#2092 = CARTESIAN_POINT ( 'NONE',  ( -15.26192592288499483, -4.160213195839838285, -314.9999999999998863 ) ) ;
#2093 = CARTESIAN_POINT ( 'NONE',  ( -5.875275055693564674, -3.272594625989450723, -436.9218166935183376 ) ) ;
#2094 = CARTESIAN_POINT ( 'NONE',  ( -17.50000000000000711, 8.653878165429867666E-10, 190.0000000000001137 ) ) ;
#2095 = EDGE_CURVE ( 'NONE', #6759, #2473, #7328, .T. ) ;
#2096 = CARTESIAN_POINT ( 'NONE',  ( -11.71572875797656188, 12.49999999864037825, -316.5000000000000000 ) ) ;
#2097 = CARTESIAN_POINT ( 'NONE',  ( -3.024115758602054171, 9.348088905657231606, -315.0000000000000000 ) ) ;
#2099 = DIRECTION ( 'NONE',  ( -0.2381566831044918675, 0.000000000000000000, 0.9712267471052610235 ) ) ;
#2098 = CIRCLE ( 'NONE', #1067, 3.499999999999998668 ) ;
#2100 = CARTESIAN_POINT ( 'NONE',  ( 11.05317456124874553, 7.762181834020175586, 314.4999466939158879 ) ) ;
#2101 = EDGE_LOOP ( 'NONE', ( #7660, #1453, #460, #3857 ) ) ;
#2102 = CARTESIAN_POINT ( 'NONE',  ( -14.32993508528999982, -7.533629911342000440, -317.5000000000000000 ) ) ;
#2103 = CARTESIAN_POINT ( 'NONE',  ( -80.80421425739181984, -2.500000000000000000, -329.3491872523243842 ) ) ;
#2104 = DIRECTION ( 'NONE',  ( 0.000000000000000000, 0.000000000000000000, 1.000000000000000000 ) ) ;
#2105 = CARTESIAN_POINT ( 'NONE',  ( 2.257382111677873393, -9.415175415973715545, 315.0000000000000000 ) ) ;
#2106 = CARTESIAN_POINT ( 'NONE',  ( 3.846123575835999731, 9.203727088275000412, -315.0848619657999734 ) ) ;
#2107 = DIRECTION ( 'NONE',  ( -0.9902680687415799099, 0.000000000000000000, -0.1391731009599969648 ) ) ;
#2108 = VECTOR ( 'NONE', #1151, 1000.000000000000000 ) ;
#2109 = CARTESIAN_POINT ( 'NONE',  ( -17.16661504264607885, 5.088157322090969144E-08, 314.8332817084517501 ) ) ;
#2110 = CARTESIAN_POINT ( 'NONE',  ( -14.83150119643293330, -5.565240525586856002, -439.0507257690958909 ) ) ;
#2111 = DIRECTION ( 'NONE',  ( 0.000000000000000000, 0.000000000000000000, -1.000000000000000000 ) ) ;
#2112 = ORIENTED_EDGE ( 'NONE', *, *, #2260, .T. ) ;
#2113 = CARTESIAN_POINT ( 'NONE',  ( -17.42196264042997100, 5.530423875593995398, -317.5770954168139610 ) ) ;
#2114 = CARTESIAN_POINT ( 'NONE',  ( -13.67588481992999228, -8.646726704586995993, -317.5770954168139610 ) ) ;
#2115 = FACE_OUTER_BOUND ( 'NONE', #7123, .T. ) ;
#2116 = CARTESIAN_POINT ( 'NONE',  ( -38.38033378105252780, -2.500000000000000000, -506.9690816445435644 ) ) ;
#2117 = ORIENTED_EDGE ( 'NONE', *, *, #1671, .F. ) ;
#2118 = SURFACE_SIDE_STYLE ('',( #9331 ) ) ;
#2119 = CARTESIAN_POINT ( 'NONE',  ( -19.99999721132999753, 3.518711422920000253E-10, 319.0000000000000000 ) ) ;
#2120 = ADVANCED_FACE ( 'NONE', ( #5600 ), #4803, .F. ) ;
#2121 = CIRCLE ( 'NONE', #9340, 12.49999999999998934 ) ;
#2122 = EDGE_LOOP ( 'NONE', ( #565, #7254, #9589, #2187 ) ) ;
#2123 = CARTESIAN_POINT ( 'NONE',  ( -19.63511402242740189, -9.000000000000001776, -416.9332195861429113 ) ) ;
#2124 = VERTEX_POINT ( 'NONE', #5758 ) ;
#2125 = CARTESIAN_POINT ( 'NONE',  ( -72.90663470102438737, 7.399494936611693774, -371.7168990826883714 ) ) ;
#2126 = CARTESIAN_POINT ( 'NONE',  ( 1.499999999999999556, 2.500000000000000000, -409.5000000000000568 ) ) ;
#2127 = CARTESIAN_POINT ( 'NONE',  ( 7.559362580479000115, 11.57734716366000072, 191.1197171614399792 ) ) ;
#2128 = ADVANCED_FACE ( 'NONE', ( #2384, #3942 ), #4100, .F. ) ;
#2129 = MECHANICAL_DESIGN_GEOMETRIC_PRESENTATION_REPRESENTATION (  '', ( #1264 ), #10532 ) ;
#2130 = CARTESIAN_POINT ( 'NONE',  ( -1.284201520726217627, -7.481087858561002335, -434.4823192484363403 ) ) ;
#2131 = ADVANCED_FACE ( 'NONE', ( #8935 ), #5707, .T. ) ;
#2132 = CARTESIAN_POINT ( 'NONE',  ( 19.46046181435998079, 1.651614223715000884, -302.4229045757450081 ) ) ;
#2133 = CARTESIAN_POINT ( 'NONE',  ( -18.27279225368999249, -5.234253896328004529, 319.5792614743400009 ) ) ;
#2134 = FACE_OUTER_BOUND ( 'NONE', #8477, .T. ) ;
#2135 = CARTESIAN_POINT ( 'NONE',  ( -13.37260572687999982, 6.041714840053000302, 314.8616023057000461 ) ) ;
#2136 = ORIENTED_EDGE ( 'NONE', *, *, #597, .T. ) ;
#2137 = CARTESIAN_POINT ( 'NONE',  ( -19.99999721801999897, -7.771324026006999692E-11, 191.0000000000000000 ) ) ;
#2138 = CARTESIAN_POINT ( 'NONE',  ( 6.472425350819999146, 11.83301930295000126, 318.8802828394900644 ) ) ;
#2139 = CARTESIAN_POINT ( 'NONE',  ( 0.000000000000000000, 0.000000000000000000, -315.0000000000000000 ) ) ;
#2140 = VECTOR ( 'NONE', #5990, 1000.000000000000000 ) ;
#2141 = CIRCLE ( 'NONE', #1449, 12.49999999999998934 ) ;
#2142 = TOROIDAL_SURFACE ( 'NONE', #4724, 15.50000000000000000, 0.5000000000000000000 ) ;
#2143 = EDGE_CURVE ( 'NONE', #4786, #9383, #9882, .T. ) ;
#2144 = DIRECTION ( 'NONE',  ( 0.000000000000000000, 1.000000000000000000, 0.000000000000000000 ) ) ;
#2145 = CARTESIAN_POINT ( 'NONE',  ( -8.518317708839887814, -7.500000000000000000, -528.6824739677025491 ) ) ;
#2146 = CARTESIAN_POINT ( 'NONE',  ( -65.06086774555899410, -12.50000000000000000, -381.4479802600495759 ) ) ;
#2147 = CARTESIAN_POINT ( 'NONE',  ( -2.814980436929585108E-10, -12.50000000000000000, 191.0000000000000000 ) ) ;
#2148 = AXIS2_PLACEMENT_3D ( 'NONE', #1982, #4493, #10142 ) ;
#2149 = CARTESIAN_POINT ( 'NONE',  ( -14.65054575295525296, -4.807282645526338882, -315.0000000000000000 ) ) ;
#2150 = CARTESIAN_POINT ( 'NONE',  ( -20.00000000000000000, -7.771159141713679452E-11, 191.0000000000000000 ) ) ;
#2151 = CARTESIAN_POINT ( 'NONE',  ( -11.57898025333339831, -5.948622255021098759, -438.8369007677023319 ) ) ;
#2152 = CARTESIAN_POINT ( 'NONE',  ( 2.157987297531679616, 9.422522223986293355, -314.9999999999999432 ) ) ;
#2153 = APPLICATION_CONTEXT ( 'automotive_design' ) ;
#2154 = CARTESIAN_POINT ( 'NONE',  ( 19.55151251130001100, 0.8490756357253000930, 189.9229057364800042 ) ) ;
#2155 = CARTESIAN_POINT ( 'NONE',  ( 15.42236153691470690, 4.758481100888916515, 314.4999482133868582 ) ) ;
#2156 = ORIENTED_EDGE ( 'NONE', *, *, #7840, .T. ) ;
#2157 = CARTESIAN_POINT ( 'NONE',  ( -6.294344443169999970, -10.85463315985999877, -317.5000000000000000 ) ) ;
#2158 = CYLINDRICAL_SURFACE ( 'NONE', #9318, 3.500000000000003109 ) ;
#2159 = DIRECTION ( 'NONE',  ( 1.000000000000000000, 0.000000000000000000, 0.000000000000000000 ) ) ;
#2160 = CARTESIAN_POINT ( 'NONE',  ( 16.84526280568076118, -1.268064982489031545, 315.0000000000000568 ) ) ;
#2161 = CARTESIAN_POINT ( 'NONE',  ( -8.759386130138000937, 8.782224002452998946, -314.4150829855000211 ) ) ;
#2162 = CARTESIAN_POINT ( 'NONE',  ( -31.51838671672000558, -2.500000000000000000, -497.7560445212000104 ) ) ;
#2163 = CARTESIAN_POINT ( 'NONE',  ( -14.51666864684999680, 8.103202762918000346, 320.0770942683900557 ) ) ;
#2164 = FACE_OUTER_BOUND ( 'NONE', #3632, .T. ) ;
#2165 = CARTESIAN_POINT ( 'NONE',  ( -0.4139159552628927652, -2.492503281179000663, -434.4399094585419903 ) ) ;
#2166 = ORIENTED_EDGE ( 'NONE', *, *, #7924, .T. ) ;
#2167 = CARTESIAN_POINT ( 'NONE',  ( 13.67588481992999228, 8.646726704586995993, -317.5770954168139610 ) ) ;
#2168 = CARTESIAN_POINT ( 'NONE',  ( -6.484736462137004942, -11.91614536315999828, -317.0792622552969533 ) ) ;
#2169 = DIRECTION ( 'NONE',  ( 0.000000000000000000, 1.000000000000000000, 0.000000000000000000 ) ) ;
#2170 = CARTESIAN_POINT ( 'NONE',  ( -17.50000000000125056, 0.2304358844820636465, -314.4997350343305129 ) ) ;
#2171 = ORIENTED_EDGE ( 'NONE', *, *, #4040, .F. ) ;
#2172 = CARTESIAN_POINT ( 'NONE',  ( -8.751711036432999080, 10.20177972100999853, 190.0000000000000000 ) ) ;
#2173 = AXIS2_PLACEMENT_3D ( 'NONE', #6893, #10160, #9209 ) ;
#2174 = CARTESIAN_POINT ( 'NONE',  ( -28.28616793536999907, -2.500000000000000000, -432.8909064497000259 ) ) ;
#2175 = ORIENTED_EDGE ( 'NONE', *, *, #7655, .T. ) ;
#2176 = CARTESIAN_POINT ( 'NONE',  ( 16.85039254115126539, 6.759165854037039622, -316.5000000000004547 ) ) ;
#2177 = ORIENTED_EDGE ( 'NONE', *, *, #2731, .F. ) ;
#2178 = CARTESIAN_POINT ( 'NONE',  ( 17.49999999911141302, -5.867334123717704131, -302.4999999999996021 ) ) ;
#2179 = CARTESIAN_POINT ( 'NONE',  ( -5.185096592093999313, -11.65847420015999170, -302.4229045757450081 ) ) ;
#2180 = CARTESIAN_POINT ( 'NONE',  ( 13.93226991011998450, 8.970845217077998868, 191.1197171614399792 ) ) ;
#2181 = CARTESIAN_POINT ( 'NONE',  ( -1.552911365449734626, -7.327055393686999984, -435.0269566445958276 ) ) ;
#2182 = CARTESIAN_POINT ( 'NONE',  ( 15.21156667173000621, 6.719223644262998008, -302.5071922382879279 ) ) ;
#2183 = PRODUCT ( 'Hinge Pin', 'Hinge Pin', '', ( #7210 ) ) ;
#2184 = CARTESIAN_POINT ( 'NONE',  ( -10.18759338605000409, -10.75836373329000217, 318.8802828394900644 ) ) ;
#2185 = CARTESIAN_POINT ( 'NONE',  ( -1.266716818501000041, -9.650794245151999462, -314.8616023057000461 ) ) ;
#2186 = CARTESIAN_POINT ( 'NONE',  ( 18.86954045039000150, 1.614942466016999978, -302.4999999999529905 ) ) ;
#2187 = ORIENTED_EDGE ( 'NONE', *, *, #1880, .F. ) ;
#2188 = CARTESIAN_POINT ( 'NONE',  ( -14.98500449093754483, -6.508849730028000380, -438.4247239981262396 ) ) ;
#2189 = CONICAL_SURFACE ( 'NONE', #6830, 3.400000000000014122, 0.7853981633975372079 ) ;
#2190 = CARTESIAN_POINT ( 'NONE',  ( -1.099124599181354522, -7.471261185735560417, -434.4594340131810100 ) ) ;
#2191 = PRODUCT_DEFINITION ( 'UNKNOWN', '', #5412, #7223 ) ;
#2192 = DIRECTION ( 'NONE',  ( 0.4712473909295827323, 0.000000000000000000, -0.8820010751365675583 ) ) ;
#2193 = DIRECTION ( 'NONE',  ( 0.000000000000000000, -1.000000000000000000, 0.000000000000000000 ) ) ;
#2194 = VECTOR ( 'NONE', #7487, 1000.000000000000114 ) ;
#2195 = CARTESIAN_POINT ( 'NONE',  ( -16.80170962578117155, 1.436180489853609688, 315.0000000000000568 ) ) ;
#2196 = CARTESIAN_POINT ( 'NONE',  ( -16.24851264371998738, -5.765366273007000331, 319.9928079742500131 ) ) ;
#2197 = CARTESIAN_POINT ( 'NONE',  ( -6.369817261971415512, -8.818538635844451079, -315.0000000000000000 ) ) ;
#2198 = CARTESIAN_POINT ( 'NONE',  ( -17.50000000088855501, -5.867334121986932161, 189.9999999999998010 ) ) ;
#2199 = CARTESIAN_POINT ( 'NONE',  ( -19.53582934753526246, -8.000000000000000000, -416.4196174530124495 ) ) ;
#2200 = EDGE_LOOP ( 'NONE', ( #9939, #4887, #2225, #2219 ) ) ;
#2201 = FACE_OUTER_BOUND ( 'NONE', #9913, .T. ) ;
#2202 = ADVANCED_FACE ( 'NONE', ( #8340 ), #10258, .T. ) ;
#2203 = CARTESIAN_POINT ( 'NONE',  ( 1.962614641415807215, 9.435987819058210491, -314.9999999999999432 ) ) ;
#2204 = CARTESIAN_POINT ( 'NONE',  ( -19.59090808375999515, 0.09664295149309998223, 189.9229057364800042 ) ) ;
#2205 = CARTESIAN_POINT ( 'NONE',  ( 1.514429654104534930E-09, 10.00000000000000000, -302.5000000000000568 ) ) ;
#2206 = ADVANCED_FACE ( 'NONE', ( #126 ), #2189, .T. ) ;
#2207 = CARTESIAN_POINT ( 'NONE',  ( -8.891587890486999157, -10.15986303230000054, -317.5000000000000000 ) ) ;
#2208 =( REPRESENTATION_RELATIONSHIP ('NONE','NONE', #8468, #33 ) REPRESENTATION_RELATIONSHIP_WITH_TRANSFORMATION ( #7524 )SHAPE_REPRESENTATION_RELATIONSHIP( ) );
#2209 = CARTESIAN_POINT ( 'NONE',  ( -102.0103468492230547, -2.500000000000000000, -289.6591388711787545 ) ) ;
#2210 =( NAMED_UNIT ( * ) PLANE_ANGLE_UNIT ( ) SI_UNIT ( $, .RADIAN. ) );
#2211 = CARTESIAN_POINT ( 'NONE',  ( 16.74588786138889063, -1.629246332199927538, 315.0000000000000000 ) ) ;
#2212 = CARTESIAN_POINT ( 'NONE',  ( 1.266716818501000041, 9.650794245151999462, -314.8616023057000461 ) ) ;
#2213 = ADVANCED_FACE ( 'NONE', ( #1948, #9905, #2651 ), #3510, .T. ) ;
#2214 = DIRECTION ( 'NONE',  ( 0.9902680687415800209, 0.000000000000000000, 0.1391731009599966873 ) ) ;
#2215 = ADVANCED_FACE ( 'NONE', ( #9151, #5919, #334 ), #7585, .F. ) ;
#2216 = CARTESIAN_POINT ( 'NONE',  ( 14.64020885817999584, 8.017619026918998415, 320.0770942683900557 ) ) ;
#2217 =( LENGTH_UNIT ( ) NAMED_UNIT ( * ) SI_UNIT ( .MILLI., .METRE. ) );
#2218 = CARTESIAN_POINT ( 'NONE',  ( -0.3413170418743253776, -2.457820343117000039, -433.9546262319294669 ) ) ;
#2219 = ORIENTED_EDGE ( 'NONE', *, *, #6388, .F. ) ;
#2220 = CARTESIAN_POINT ( 'NONE',  ( 18.86307259346999032, -0.4762574081846996932, -317.4928077629770087 ) ) ;
#2221 = CARTESIAN_POINT ( 'NONE',  ( 10.59417419979999586, -10.60664446758999446, -316.3802825947000201 ) ) ;
#2222 = CIRCLE ( 'NONE', #6884, 4.000000000000009770 ) ;
#2223 = LINE ( 'NONE', #6352, #6367 ) ;
#2224 = CARTESIAN_POINT ( 'NONE',  ( -16.39269942312257200, 3.424609558409217325, -314.5540176726823347 ) ) ;
#2225 = ORIENTED_EDGE ( 'NONE', *, *, #704, .F. ) ;
#2226 = CIRCLE ( 'NONE', #2050, 0.5000000000000004441 ) ;
#2227 = FACE_OUTER_BOUND ( 'NONE', #997, .T. ) ;
#2228 = ADVANCED_FACE ( 'NONE', ( #1789 ), #9211, .F. ) ;
#2229 = ORIENTED_EDGE ( 'NONE', *, *, #7954, .F. ) ;
#2230 = CARTESIAN_POINT ( 'NONE',  ( 11.66810544104021297, 10.16551412172561442, -316.5000000000004547 ) ) ;
#2231 = EDGE_LOOP ( 'NONE', ( #5461, #1677, #4432, #9762 ) ) ;
#2232 = CARTESIAN_POINT ( 'NONE',  ( -12.11102551177084941, -6.646503028198875285, 314.9999999999999432 ) ) ;
#2233 = CARTESIAN_POINT ( 'NONE',  ( -16.55370135034999990, -6.459991253353003948, -302.4229045757450081 ) ) ;
#2234 = DIRECTION ( 'NONE',  ( 0.000000000000000000, -1.000000000000000000, 0.000000000000000000 ) ) ;
#2235 = AXIS2_PLACEMENT_3D ( 'NONE', #787, #9063, #3473 ) ;
#2236 = CARTESIAN_POINT ( 'NONE',  ( 15.65461689722998706, 7.260828390490999595, -302.4229045757450081 ) ) ;
#2237 = CARTESIAN_POINT ( 'NONE',  ( -19.00000000000000000, 0.000000000000000000, -302.5000000001010108 ) ) ;
#2238 = ORIENTED_EDGE ( 'NONE', *, *, #3036, .T. ) ;
#2239 = CARTESIAN_POINT ( 'NONE',  ( 8.759386130138000937, -8.782224002452998946, -314.4150829855000211 ) ) ;
#2240 = CARTESIAN_POINT ( 'NONE',  ( -17.50000000000000711, 8.653878165429867666E-10, 190.0000000000001137 ) ) ;
#2241 = ORIENTED_EDGE ( 'NONE', *, *, #6861, .F. ) ;
#2242 = CARTESIAN_POINT ( 'NONE',  ( 19.10187173594998811, -2.686732971880998910, 189.9229057364800042 ) ) ;
#2243 = CARTESIAN_POINT ( 'NONE',  ( -2.000000000000000000, -10.50000000000000000, -409.5000000000000000 ) ) ;
#2244 = AXIS2_PLACEMENT_3D ( 'NONE', #6985, #4554, #7828 ) ;
#2245 = DIRECTION ( 'NONE',  ( 0.9958031466069998672, 0.000000000000000000, 0.09152099872487109988 ) ) ;
#2246 = ADVANCED_FACE ( 'NONE', ( #8391 ), #6842, .F. ) ;
#2247 = VERTEX_POINT ( 'NONE', #978 ) ;
#2248 = CARTESIAN_POINT ( 'NONE',  ( -14.23799507159000122, -5.083276007328000112, 315.0848619657999734 ) ) ;
#2249 = CARTESIAN_POINT ( 'NONE',  ( -2.000000000000000000, -9.500000000000000000, -404.4999999999999432 ) ) ;
#2250 = LINE ( 'NONE', #3164, #3772 ) ;
#2251 = CARTESIAN_POINT ( 'NONE',  ( -3.309734165293447550, -9.320883339027414394, -315.0000000000000568 ) ) ;
#2252 = CARTESIAN_POINT ( 'NONE',  ( -10.23467949917771591, -9.999999999493891067, 189.9999999999997726 ) ) ;
#2253 = LINE ( 'NONE', #9026, #6422 ) ;
#2254 = ORIENTED_EDGE ( 'NONE', *, *, #9718, .F. ) ;
#2255 = CARTESIAN_POINT ( 'NONE',  ( -72.90663470102438737, -2.500000000000000444, -375.1168990826883487 ) ) ;
#2256 = ADVANCED_FACE ( 'NONE', ( #4368 ), #3045, .T. ) ;
#2257 = CARTESIAN_POINT ( 'NONE',  ( -15.66663193639001506, 7.880331994043005217, 190.4207385301700128 ) ) ;
#2258 = CARTESIAN_POINT ( 'NONE',  ( -13.30825372127758399, -8.000000000000000000, -400.6612558711213410 ) ) ;
#2259 = PLANE ( 'NONE',  #5785 ) ;
#2260 = EDGE_CURVE ( 'NONE', #5868, #10390, #7313, .T. ) ;
#2261 = DIRECTION ( 'NONE',  ( -0.8820010751365675583, 0.000000000000000000, -0.4712473909295827323 ) ) ;
#2262 = DIRECTION ( 'NONE',  ( 0.5469441386039887165, 7.874726160959139460E-17, -0.8371691043312221581 ) ) ;
#2263 = CARTESIAN_POINT ( 'NONE',  ( 0.000000000000000000, 10.54711710274999881, -315.0000000000000000 ) ) ;
#2264 = EDGE_CURVE ( 'NONE', #3224, #3141, #2026, .T. ) ;
#2265 = CARTESIAN_POINT ( 'NONE',  ( 16.07469914181999826, 3.754035329064000059, -314.6383426456000052 ) ) ;
#2266 = LINE ( 'NONE', #5533, #6349 ) ;
#2267 = CIRCLE ( 'NONE', #8270, 3.499999999999997335 ) ;
#2268 = CARTESIAN_POINT ( 'NONE',  ( -18.44593188493998426, 2.441603908132000011, 319.9928079742500131 ) ) ;
#2269 = FACE_OUTER_BOUND ( 'NONE', #4438, .T. ) ;
#2270 = CARTESIAN_POINT ( 'NONE',  ( -1.170915164613087756, -2.622174536531001188, -434.8787092738958791 ) ) ;
#2271 = ORIENTED_EDGE ( 'NONE', *, *, #694, .T. ) ;
#2272 = CARTESIAN_POINT ( 'NONE',  ( -18.63147570264002084, 4.749337304460001796, -317.0792622552969533 ) ) ;
#2273 = CARTESIAN_POINT ( 'NONE',  ( 13.93264803488000858, -8.974986968055002734, -316.3802825947000201 ) ) ;
#2274 = ORIENTED_EDGE ( 'NONE', *, *, #5034, .T. ) ;
#2275 = CARTESIAN_POINT ( 'NONE',  ( 2.579601697407999605, -11.41110358643000033, 320.0000000000000000 ) ) ;
#2276 = EDGE_CURVE ( 'NONE', #8515, #5739, #3659, .T. ) ;
#2277 = AXIS2_PLACEMENT_3D ( 'NONE', #9985, #7618, #6655 ) ;
#2278 = UNCERTAINTY_MEASURE_WITH_UNIT (LENGTH_MEASURE( 1.000000000000000082E-05 ), #10040, 'distance_accuracy_value', 'NONE');
#2279 = DIRECTION ( 'NONE',  ( -2.716996281154024841E-06, 0.9999999999963090636, 1.474966429758616062E-22 ) ) ;
#2280 = DIRECTION ( 'NONE',  ( -0.1071946444232947937, 0.000000000000000000, 0.9942380540931651245 ) ) ;
#2281 = ORIENTED_EDGE ( 'NONE', *, *, #757, .F. ) ;
#2282 = CARTESIAN_POINT ( 'NONE',  ( -11.52006393673609885, -7.476351274249519285, -314.5677505184611391 ) ) ;
#2283 = ORIENTED_EDGE ( 'NONE', *, *, #1436, .F. ) ;
#2284 = CARTESIAN_POINT ( 'NONE',  ( -72.90663470096859555, -2.500000000000000000, -371.7168990827444190 ) ) ;
#2285 = ORIENTED_EDGE ( 'NONE', *, *, #235, .F. ) ;
#2286 = CARTESIAN_POINT ( 'NONE',  ( -14.44906369208900365, -4.983045831585199537, 315.0000000000000568 ) ) ;
#2287 = CARTESIAN_POINT ( 'NONE',  ( 19.46926817186999514, -1.611439533454998241, -302.4229045757450081 ) ) ;
#2288 = DIRECTION ( 'NONE',  ( 0.000000000000000000, 1.000000000000000000, 0.000000000000000000 ) ) ;
#2289 = ORIENTED_EDGE ( 'NONE', *, *, #9983, .F. ) ;
#2290 = CARTESIAN_POINT ( 'NONE',  ( 1.988818824435997890, 12.53224469152999099, -302.9207377450070453 ) ) ;
#2291 = VECTOR ( 'NONE', #585, 1000.000000000000000 ) ;
#2292 = CARTESIAN_POINT ( 'NONE',  ( -13.15302580975001234, -9.418553998452996012, 318.8802828394900644 ) ) ;
#2293 = VERTEX_POINT ( 'NONE', #8541 ) ;
#2294 = CARTESIAN_POINT ( 'NONE',  ( -6.322301096779000318, -8.991223814764000011, -314.8616023057000461 ) ) ;
#2295 = CARTESIAN_POINT ( 'NONE',  ( -1.813125407131493949, -2.572135581867000198, -434.7536649739391237 ) ) ;
#2296 = ORIENTED_EDGE ( 'NONE', *, *, #6736, .F. ) ;
#2297 = CARTESIAN_POINT ( 'NONE',  ( -16.23266328071998643, -5.782092517776998619, 190.0071920248299477 ) ) ;
#2298 = CARTESIAN_POINT ( 'NONE',  ( -19.49681644515301215, 2.834072041603171499, 190.9999999999996589 ) ) ;
#2299 = CARTESIAN_POINT ( 'NONE',  ( -46.74071243416547361, -2.500000000000000000, -414.3237589990478114 ) ) ;
#2300 = COLOUR_RGB ( '', 0.09019608, 0.27058824, 0.51372549) ;
#2301 = CARTESIAN_POINT ( 'NONE',  ( -8.655660348039997842, -8.816209662726999241, 314.4150829855000211 ) ) ;
#2302 = CARTESIAN_POINT ( 'NONE',  ( -46.74071243416547361, -7.500000000000000000, -414.3237589990478114 ) ) ;
#2303 = DIRECTION ( 'NONE',  ( 0.7508065140037780694, 0.000000000000000000, -0.6605222013903048195 ) ) ;
#2304 = CARTESIAN_POINT ( 'NONE',  ( -15.54870946350325767, -7.500000000000000000, -436.1258788022018393 ) ) ;
#2305 = CIRCLE ( 'NONE', #1040, 3.500000000000003997 ) ;
#2306 = CARTESIAN_POINT ( 'NONE',  ( 3.205490369836122788, 12.35619803902316960, 319.0000000000005116 ) ) ;
#2307 = DIRECTION ( 'NONE',  ( 0.000000000000000000, -1.000000000000000000, 0.000000000000000000 ) ) ;
#2308 = CARTESIAN_POINT ( 'NONE',  ( -15.00000000000000000, 0.000000000000000000, 315.0000000000000000 ) ) ;
#2309 = VECTOR ( 'NONE', #9307, 1000.000000000000114 ) ;
#2310 = EDGE_LOOP ( 'NONE', ( #7345, #2928, #3923, #8777 ) ) ;
#2311 = FACE_OUTER_BOUND ( 'NONE', #7175, .T. ) ;
#2312 = CIRCLE ( 'NONE', #8147, 15.00000000000001776 ) ;
#2313 = CARTESIAN_POINT ( 'NONE',  ( 6.027267673561996553, 11.50416862954998365, 189.9229057364800042 ) ) ;
#2314 = CARTESIAN_POINT ( 'NONE',  ( -10.23467949614885697, 10.00000000050611781, 189.9999999999995737 ) ) ;
#2315 = CYLINDRICAL_SURFACE ( 'NONE', #3737, 3.500000000000006217 ) ;
#2316 = AXIS2_PLACEMENT_3D ( 'NONE', #7503, #9874, #37 ) ;
#2317 = EDGE_CURVE ( 'NONE', #6229, #4674, #6126, .T. ) ;
#2318 = DIRECTION ( 'NONE',  ( 0.000000000000000000, 1.000000000000000000, -0.000000000000000000 ) ) ;
#2319 = APPLICATION_PROTOCOL_DEFINITION ( 'draft international standard', 'automotive_design', 1998, #9633 ) ;
#2320 = CARTESIAN_POINT ( 'NONE',  ( -5.255569329967309855, -12.07344867603089256, -303.5000000000006253 ) ) ;
#2321 = CARTESIAN_POINT ( 'NONE',  ( 16.54291557298000370, 1.991497705781999805, -315.0848619657999734 ) ) ;
#2322 =( NAMED_UNIT ( * ) PLANE_ANGLE_UNIT ( ) SI_UNIT ( $, .RADIAN. ) );
#2323 = CARTESIAN_POINT ( 'NONE',  ( 19.55138120870000407, 0.8505817651195003437, 320.0770942683900557 ) ) ;
#2324 = CARTESIAN_POINT ( 'NONE',  ( -26.82908671702000802, -2.500000000000000000, -441.1544246730000509 ) ) ;
#2325 = ORIENTED_EDGE ( 'NONE', *, *, #2474, .F. ) ;
#2326 = CARTESIAN_POINT ( 'NONE',  ( -1.897969053490322855, -2.548986172702000896, -434.7293254325074940 ) ) ;
#2327 = ORIENTED_EDGE ( 'NONE', *, *, #5504, .F. ) ;
#2328 = CARTESIAN_POINT ( 'NONE',  ( 19.56018598331999314, -0.5259244641825996380, -317.5770954168139610 ) ) ;
#2329 = DIRECTION ( 'NONE',  ( 0.000000000000000000, -1.000000000000000000, 0.000000000000000000 ) ) ;
#2330 = EDGE_CURVE ( 'NONE', #863, #1584, #7052, .T. ) ;
#2331 = PRESENTATION_LAYER_ASSIGNMENT (  '', '', ( #4555 ) ) ;
#2332 = DIRECTION ( 'NONE',  ( 0.000000000000000000, 0.000000000000000000, 1.000000000000000000 ) ) ;
#2333 = VERTEX_POINT ( 'NONE', #2805 ) ;
#2334 = CARTESIAN_POINT ( 'NONE',  ( 0.000000000000000000, 0.000000000000000000, 190.0000000000000000 ) ) ;
#2335 = FACE_OUTER_BOUND ( 'NONE', #5716, .T. ) ;
#2336 = ORIENTED_EDGE ( 'NONE', *, *, #1553, .T. ) ;
#2337 = CARTESIAN_POINT ( 'NONE',  ( 10.00000000000000000, 2.500000000000000000, -272.5000000000000000 ) ) ;
#2338 = ORIENTED_EDGE ( 'NONE', *, *, #3580, .T. ) ;
#2339 = DIRECTION ( 'NONE',  ( -0.2951854283188052319, 0.000000000000000000, 0.9554399839384175586 ) ) ;
#2340 = ORIENTED_EDGE ( 'NONE', *, *, #36, .F. ) ;
#2341 = CARTESIAN_POINT ( 'NONE',  ( -4.669690493011572130, -9.131031402067035785, 315.0000000000001137 ) ) ;
#2342 = CARTESIAN_POINT ( 'NONE',  ( -0.1642067852079997503, -12.59486910148998895, -302.9207377450070453 ) ) ;
#2343 = EDGE_CURVE ( 'NONE', #3286, #7297, #651, .T. ) ;
#2344 = DIRECTION ( 'NONE',  ( 0.000000000000000000, -1.000000000000000000, 0.000000000000000000 ) ) ;
#2345 = B_SPLINE_CURVE_WITH_KNOTS ( 'NONE', 3,
 ( #1748, #250, #9010, #89, #8197, #5824, #3366, #6643, #9918, #2555, #9116, #10178 ),
 .UNSPECIFIED., .F., .F.,
 ( 4, 2, 2, 2, 2, 4 ),
 ( 0.000000000000000000, 0.06249999999999888978, 0.1249999999999977796, 0.2499999999999998890, 0.4999999999999998890, 1.000000000000000000 ),
 .UNSPECIFIED. ) ;
#2346 = EDGE_CURVE ( 'NONE', #5580, #3896, #652, .T. ) ;
#2347 = CARTESIAN_POINT ( 'NONE',  ( 11.28781796570999951, -4.951468039558000633, 315.0000000000000000 ) ) ;
#2348 = FILL_AREA_STYLE_COLOUR ( '', #10564 ) ;
#2349 = CARTESIAN_POINT ( 'NONE',  ( -11.75341581114999023, 10.21170493764999598, -302.9207377450070453 ) ) ;
#2350 = LINE ( 'NONE', #8952, #5308 ) ;
#2351 = ORIENTED_EDGE ( 'NONE', *, *, #5085, .T. ) ;
#2352 = CARTESIAN_POINT ( 'NONE',  ( -14.38384290288000145, -5.252906928686999599, -314.8616023057000461 ) ) ;
#2353 = EDGE_CURVE ( 'NONE', #56, #5548, #474, .T. ) ;
#2354 = CARTESIAN_POINT ( 'NONE',  ( -2.971092673426039443, -2.641283117323076191, -435.1576634133632524 ) ) ;
#2355 = EDGE_LOOP ( 'NONE', ( #1475, #275, #5041, #1037 ) ) ;
#2356 = CARTESIAN_POINT ( 'NONE',  ( 9.985646804708002477, -10.39189181891999780, 189.9229057364800042 ) ) ;
#2357 = CARTESIAN_POINT ( 'NONE',  ( -17.62182611535274290, 5.928443937941890063, 190.9999999999996589 ) ) ;
#2358 = CYLINDRICAL_SURFACE ( 'NONE', #6355, 11.00000000000000000 ) ;
#2359 = CARTESIAN_POINT ( 'NONE',  ( 1.409290114754000012, -9.868237606049000021, 314.6383426456000052 ) ) ;
#2360 = CARTESIAN_POINT ( 'NONE',  ( 10.32803372116435270, 10.00000000000000178, 315.0000000000000000 ) ) ;
#2361 = DIRECTION ( 'NONE',  ( 0.000000000000000000, 1.000000000000000000, 0.000000000000000000 ) ) ;
#2362 = CARTESIAN_POINT ( 'NONE',  ( -16.80239380511999059, -5.162410948549997158, 319.9928079742500131 ) ) ;
#2363 = FACE_OUTER_BOUND ( 'NONE', #186, .T. ) ;
#2364 = B_SPLINE_CURVE_WITH_KNOTS ( 'NONE', 3,
 ( #8051, #7252, #5630, #3921, #3869, #8746, #5578, #4027, #4081, #8860, #7146, #10579, #10520, #1502, #4784, #3222, #1444, #6384 ),
 .UNSPECIFIED., .F., .F.,
 ( 4, 1, 1, 1, 1, 2, 2, 1, 1, 2, 2, 4 ),
 ( 0.000000000000000000, 0.2499999999994746425, 0.3749999999992318367, 0.4374999999991385780, 0.4687499999990925592, 0.4843749999990695221, 0.4999999999990465405, 0.6249999999991870947, 0.6874999999993030020, 0.7187499999993127719, 0.7499999999993226529, 1.000000000000000000 ),
 .UNSPECIFIED. ) ;
#2365 = CARTESIAN_POINT ( 'NONE',  ( -2.000000000000000000, 3.500000000000000000, -404.4999999999999432 ) ) ;
#2366 = ORIENTED_EDGE ( 'NONE', *, *, #8488, .T. ) ;
#2367 = CARTESIAN_POINT ( 'NONE',  ( -1.873948611767810357, -2.500000000000000000, -349.2478646809746579 ) ) ;
#2368 = EDGE_CURVE ( 'NONE', #7412, #1407, #7005, .T. ) ;
#2369 = CARTESIAN_POINT ( 'NONE',  ( 4.407678726681998782, 11.78447947993998390, 189.9229057364800042 ) ) ;
#2370 = CARTESIAN_POINT ( 'NONE',  ( -34.39269738225353024, -2.500000000000000000, -407.7262955260336525 ) ) ;
#2371 = AXIS2_PLACEMENT_3D ( 'NONE', #9691, #5542, #3132 ) ;
#2372 = LINE ( 'NONE', #7314, #10423 ) ;
#2373 = CARTESIAN_POINT ( 'NONE',  ( -34.37192209820132405, -7.500000000000000000, -461.0868123482146643 ) ) ;
#2374 = PRODUCT_CONTEXT ( 'NONE', #6331, 'mechanical' ) ;
#2375 = CARTESIAN_POINT ( 'NONE',  ( 19.99979308783253273, -0.5741528085765136291, -303.4999999999998295 ) ) ;
#2376 = DIRECTION ( 'NONE',  ( -1.908117741397742798E-11, 1.000000000000000000, -2.057253813257758150E-12 ) ) ;
#2377 = FILL_AREA_STYLE ('',( #9036 ) ) ;
#2378 = CARTESIAN_POINT ( 'NONE',  ( -2.975649281827347448, -7.138022370016234852, -435.8156820327864693 ) ) ;
#2379 = CARTESIAN_POINT ( 'NONE',  ( 16.43550475785002263, 7.239471399781003846, 319.5792614743400009 ) ) ;
#2380 = CARTESIAN_POINT ( 'NONE',  ( -0.8018440996563184209, -2.556536707011997311, -434.4710415144371041 ) ) ;
#2381 = EDGE_LOOP ( 'NONE', ( #7557, #8525, #10280, #4646, #1829 ) ) ;
#2382 = CARTESIAN_POINT ( 'NONE',  ( 19.29920617650999404, 3.385971943253997640, -316.3802825947000201 ) ) ;
#2383 = LINE ( 'NONE', #7908, #3600 ) ;
#2384 = FACE_BOUND ( 'NONE', #9863, .T. ) ;
#2385 = CARTESIAN_POINT ( 'NONE',  ( -0.3206729354815163191, -7.530925261025000594, -434.2912207255791373 ) ) ;
#2386 = DIRECTION ( 'NONE',  ( 0.000000000000000000, 1.000000000000000000, 0.000000000000000000 ) ) ;
#2387 = PRODUCT_DEFINITION ( 'UNKNOWN', '', #3704, #870 ) ;
#2388 = CARTESIAN_POINT ( 'NONE',  ( -15.84610571802258150, 4.157530358492048883, -314.5664817403811639 ) ) ;
#2389 = EDGE_LOOP ( 'NONE', ( #6696, #4034, #7884, #9897 ) ) ;
#2390 = CARTESIAN_POINT ( 'NONE',  ( 7.495586483745385387, -11.60098025501653751, 319.0000000000003979 ) ) ;
#2391 = ORIENTED_EDGE ( 'NONE', *, *, #4577, .F. ) ;
#2392 = CARTESIAN_POINT ( 'NONE',  ( 19.86381236214655033, 1.775476277371076828, -316.5000000000004547 ) ) ;
#2393 = ORIENTED_EDGE ( 'NONE', *, *, #3216, .F. ) ;
#2394 = CARTESIAN_POINT ( 'NONE',  ( -14.02825138570089081, -5.340904894142199488, 315.0000000000000568 ) ) ;
#2395 = CARTESIAN_POINT ( 'NONE',  ( -1.957937398543000418, -12.03510449230999768, -302.4229045757450081 ) ) ;
#2396 = CARTESIAN_POINT ( 'NONE',  ( -43.24071243418999444, -2.500000000000000000, -414.3237589990000629 ) ) ;
#2397 = CARTESIAN_POINT ( 'NONE',  ( -5.563766465756743607, -8.000000000000000000, -337.3048648817380126 ) ) ;
#2398 = EDGE_CURVE ( 'NONE', #4571, #10392, #1848, .T. ) ;
#2399 = CARTESIAN_POINT ( 'NONE',  ( -16.59121592455001348, 6.423372090527998068, -302.4229045757450081 ) ) ;
#2400 = CARTESIAN_POINT ( 'NONE',  ( 10.97158218462999457, -10.45285060525999121, 318.8802828394900644 ) ) ;
#2401 = EDGE_LOOP ( 'NONE', ( #2136, #9614, #2229, #5792 ) ) ;
#2402 = CARTESIAN_POINT ( 'NONE',  ( 4.031301020048999817, -9.630010295875997883, -314.6383426456000052 ) ) ;
#2403 = CARTESIAN_POINT ( 'NONE',  ( 19.00000000000000000, 0.000000000000000000, -302.5000000001010108 ) ) ;
#2404 = ORIENTED_EDGE ( 'NONE', *, *, #1426, .T. ) ;
#2405 = CARTESIAN_POINT ( 'NONE',  ( 18.32859070493001852, -4.258570244206002720, 189.9229057364800042 ) ) ;
#2406 = CARTESIAN_POINT ( 'NONE',  ( 19.99999721801999897, 7.771189452710000131E-11, 191.0000000000000000 ) ) ;
#2407 = CARTESIAN_POINT ( 'NONE',  ( -12.45686666771074513, 6.446195019498007994, -315.0000000000000568 ) ) ;
#2408 = CARTESIAN_POINT ( 'NONE',  ( -50.43337757792475173, -7.500000000000000000, -464.9351226150769207 ) ) ;
#2409 = AXIS2_PLACEMENT_3D ( 'NONE', #10577, #745, #5681 ) ;
#2410 = EDGE_CURVE ( 'NONE', #4588, #6311, #9403, .T. ) ;
#2411 = CARTESIAN_POINT ( 'NONE',  ( -8.587332113755000051, -8.603326289371000968, 314.6383426456000052 ) ) ;
#2412 =( NAMED_UNIT ( * ) PLANE_ANGLE_UNIT ( ) SI_UNIT ( $, .RADIAN. ) );
#2413 = ADVANCED_FACE ( 'NONE', ( #6394 ), #2315, .F. ) ;
#2414 = CARTESIAN_POINT ( 'NONE',  ( -13.36276382026999876, 8.154196903800000840, 320.0000000000000000 ) ) ;
#2415 = PLANE ( 'NONE',  #9955 ) ;
#2416 = DIRECTION ( 'NONE',  ( -1.000000000000000000, 0.000000000000000000, 0.000000000000000000 ) ) ;
#2417 = CARTESIAN_POINT ( 'NONE',  ( 17.50000000000001776, -8.653793959161173735E-10, -302.4999999999998863 ) ) ;
#2418 = LINE ( 'NONE', #6552, #7791 ) ;
#2419 = CIRCLE ( 'NONE', #1901, 10.00000000000000533 ) ;
#2420 = ORIENTED_EDGE ( 'NONE', *, *, #9961, .T. ) ;
#2421 = CARTESIAN_POINT ( 'NONE',  ( 15.00000000000000000, 0.4945770392355999800, -285.0000000000000000 ) ) ;
#2422 = CIRCLE ( 'NONE', #7053, 1.999999999999998224 ) ;
#2423 = CARTESIAN_POINT ( 'NONE',  ( 20.00000000435078107, -7.322330466941333604, -303.4999999999999432 ) ) ;
#2424 = CARTESIAN_POINT ( 'NONE',  ( 15.45559681510979466, 3.931366100772827998, 315.0000000000000000 ) ) ;
#2425 = DIRECTION ( 'NONE',  ( -0.4712473909295825658, 0.000000000000000000, 0.8820010751365676693 ) ) ;
#2426 = CARTESIAN_POINT ( 'NONE',  ( 19.99999035944999903, -7.277437094418000096E-10, -303.5000000000000000 ) ) ;
#2427 = CARTESIAN_POINT ( 'NONE',  ( -12.33444409538000031, -8.732262621622000509, -302.5000000000000000 ) ) ;
#2428 =( NAMED_UNIT ( * ) SI_UNIT ( $, .STERADIAN. ) SOLID_ANGLE_UNIT ( ) );
#2429 = CARTESIAN_POINT ( 'NONE',  ( -3.355145859302810507, -7.083804960661745476, -435.9754648412450138 ) ) ;
#2430 = CARTESIAN_POINT ( 'NONE',  ( -17.04863675780999088, 6.660280422001000566, 319.5792614743400009 ) ) ;
#2431 = DIRECTION ( 'NONE',  ( 0.000000000000000000, -1.000000000000000000, 0.000000000000000000 ) ) ;
#2432 = CARTESIAN_POINT ( 'NONE',  ( -16.98100918689000238, 2.500000000000000000, -439.4179428962999623 ) ) ;
#2433 = DIRECTION ( 'NONE',  ( -0.8820010751365675583, 0.000000000000000000, -0.4712473909295825103 ) ) ;
#2434 = CARTESIAN_POINT ( 'NONE',  ( 19.98383894087000812, -0.4026063077914996402, -316.3802825947000201 ) ) ;
#2435 = CARTESIAN_POINT ( 'NONE',  ( -72.90663470102438737, -2.500000000000000000, -371.7168990826883714 ) ) ;
#2436 = ORIENTED_EDGE ( 'NONE', *, *, #7339, .F. ) ;
#2437 = CARTESIAN_POINT ( 'NONE',  ( -12.63876572971000023, -8.567575428377999458, 320.0000000000000000 ) ) ;
#2438 = CARTESIAN_POINT ( 'NONE',  ( -0.1525530514593775588, -7.663337276471000159, -433.9190241679935411 ) ) ;
#2439 = VECTOR ( 'NONE', #3583, 1000.000000000000000 ) ;
#2440 = CARTESIAN_POINT ( 'NONE',  ( -0.5691333845031163463, -2.499999797932000334, -434.2421446687361026 ) ) ;
#2441 = CARTESIAN_POINT ( 'NONE',  ( 14.89798725392377143, -4.565017050278198596, -314.9999999999999432 ) ) ;
#2442 = EDGE_LOOP ( 'NONE', ( #8291, #3143, #9082, #10187 ) ) ;
#2443 = CARTESIAN_POINT ( 'NONE',  ( 16.39269942312257911, -3.424609558409206223, -314.5540176726823347 ) ) ;
#2444 = ORIENTED_EDGE ( 'NONE', *, *, #9718, .T. ) ;
#2445 = FACE_OUTER_BOUND ( 'NONE', #1155, .T. ) ;
#2446 = ORIENTED_EDGE ( 'NONE', *, *, #3484, .T. ) ;
#2447 = CARTESIAN_POINT ( 'NONE',  ( -53.50011725782000127, -2.500000000000000000, -412.5186446566000313 ) ) ;
#2448 = DIRECTION ( 'NONE',  ( 0.4885878099338311631, 0.000000000000000000, 0.8725147288063752615 ) ) ;
#2449 = AXIS2_PLACEMENT_3D ( 'NONE', #2627, #2519, #2732 ) ;
#2450 = FACE_OUTER_BOUND ( 'NONE', #7648, .T. ) ;
#2451 = EDGE_CURVE ( 'NONE', #24, #10408, #6657, .T. ) ;
#2452 = CARTESIAN_POINT ( 'NONE',  ( 10.38823308980000704, 10.24279834975000192, -302.4229045757450081 ) ) ;
#2453 = PLANE ( 'NONE',  #3611 ) ;
#2454 = ORIENTED_EDGE ( 'NONE', *, *, #2095, .T. ) ;
#2455 = CARTESIAN_POINT ( 'NONE',  ( -16.77099092997999819, -1.279831385791999843, -315.0848619657999734 ) ) ;
#2456 = CARTESIAN_POINT ( 'NONE',  ( -14.35075321877000043, 7.519064610420000072, -302.5000000000000000 ) ) ;
#2457 = VECTOR ( 'NONE', #2065, 1000.000000000000000 ) ;
#2458 = EDGE_LOOP ( 'NONE', ( #2524, #2156, #10620, #10470 ) ) ;
#2459 = CARTESIAN_POINT ( 'NONE',  ( -18.35205128653998230, -4.220047386950002810, 189.9229057364800042 ) ) ;
#2460 = LINE ( 'NONE', #96, #9501 ) ;
#2461 = CARTESIAN_POINT ( 'NONE',  ( 14.25125116527599545, 5.161338287358923971, -315.0000000000000568 ) ) ;
#2462 = CARTESIAN_POINT ( 'NONE',  ( -10.00000000000000000, 2.500000000000000000, -285.0000000000000000 ) ) ;
#2463 = EDGE_CURVE ( 'NONE', #1779, #3477, #1511, .T. ) ;
#2464 = EDGE_CURVE ( 'NONE', #863, #8555, #9746, .T. ) ;
#2465 = CARTESIAN_POINT ( 'NONE',  ( 6.537559671572000575, -9.400791339334000796, 314.4150829855000211 ) ) ;
#2466 = CARTESIAN_POINT ( 'NONE',  ( -43.33032886859687949, -9.000000000000001776, -402.2979831847329706 ) ) ;
#2467 = CARTESIAN_POINT ( 'NONE',  ( -14.64020885817999584, -8.017619026918998415, 320.0770942683900557 ) ) ;
#2468 = FACE_OUTER_BOUND ( 'NONE', #6148, .T. ) ;
#2469 = CARTESIAN_POINT ( 'NONE',  ( 13.88908508137762432, 9.009716997455479159, -303.5000000000000000 ) ) ;
#2470 = FACE_OUTER_BOUND ( 'NONE', #8150, .T. ) ;
#2471 = ORIENTED_EDGE ( 'NONE', *, *, #10174, .F. ) ;
#2472 = DIRECTION ( 'NONE',  ( 0.000000000000000000, -1.000000000000000000, 0.000000000000000000 ) ) ;
#2473 = VERTEX_POINT ( 'NONE', #4891 ) ;
#2474 = EDGE_CURVE ( 'NONE', #7593, #3224, #2372, .T. ) ;
#2475 = CIRCLE ( 'NONE', #9348, 3.500000000000000000 ) ;
#2476 = DIRECTION ( 'NONE',  ( 2.558226600336915673E-07, -0.9999999999999674705, 3.955942811920841838E-22 ) ) ;
#2477 = CARTESIAN_POINT ( 'NONE',  ( -17.50000000000000000, 0.000000000000000000, -314.4999343908002061 ) ) ;
#2478 = CONTEXT_DEPENDENT_SHAPE_REPRESENTATION ( #3306, #9563 ) ;
#2479 = LINE ( 'NONE', #807, #4117 ) ;
#2480 = CARTESIAN_POINT ( 'NONE',  ( 16.77099092997999819, 1.279831385791999843, -315.0848619657999734 ) ) ;
#2481 = CLOSED_SHELL ( 'NONE', ( #6399, #2037, #5406, #10272, #3571, #4819, #505, #7275, #10422, #2202, #8950, #8172, #9099, #1013, #6359, #4140, #329, #1921, #3048, #6808, #3575, #4250, #9302, #9900, #9238, #477, #8750, #10156, #1328, #7265, #318, #5097, #8841, #8169 ) ) ;
#2482 = CARTESIAN_POINT ( 'NONE',  ( -19.68871134463705985, -7.500000000000000888, -416.4361005590961327 ) ) ;
#2483 = CARTESIAN_POINT ( 'NONE',  ( -17.34597251029000375, 4.674348096672999553, 190.0000000000000000 ) ) ;
#2484 = CARTESIAN_POINT ( 'NONE',  ( -14.98500449093754483, -6.508849730028000380, -438.4247239981262396 ) ) ;
#2485 = FACE_OUTER_BOUND ( 'NONE', #5432, .T. ) ;
#2486 = EDGE_LOOP ( 'NONE', ( #8430, #75, #5442, #5537 ) ) ;
#2487 = CARTESIAN_POINT ( 'NONE',  ( 20.10111883311001080, 0.3733660053931999734, -317.0792622552969533 ) ) ;
#2488 = CARTESIAN_POINT ( 'NONE',  ( -38.85901494634669007, -12.49999999999899991, -386.6556615250812570 ) ) ;
#2489 = CIRCLE ( 'NONE', #3689, 12.50000000000001421 ) ;
#2490 = VECTOR ( 'NONE', #4188, 1000.000000000000000 ) ;
#2491 = CIRCLE ( 'NONE', #1112, 3.499999999999999112 ) ;
#2492 = CARTESIAN_POINT ( 'NONE',  ( 8.531707904373998730, -10.27069628977000093, 320.0000000000000000 ) ) ;
#2493 = ORIENTED_EDGE ( 'NONE', *, *, #8386, .T. ) ;
#2494 = CARTESIAN_POINT ( 'NONE',  ( -1.219008076252173778, -7.371161895518000939, -434.8982261995575413 ) ) ;
#2495 = CARTESIAN_POINT ( 'NONE',  ( -34.37192209820132405, -7.500000000000000000, -461.0868123482146643 ) ) ;
#2496 = CARTESIAN_POINT ( 'NONE',  ( 3.024115758602054171, -9.348088905657229830, -315.0000000000000568 ) ) ;
#2497 = ORIENTED_EDGE ( 'NONE', *, *, #7977, .T. ) ;
#2498 = CARTESIAN_POINT ( 'NONE',  ( 17.19853431800999743, 2.231396706187000145, -315.0000000000001137 ) ) ;
#2499 = VERTEX_POINT ( 'NONE', #1564 ) ;
#2500 = CARTESIAN_POINT ( 'NONE',  ( 17.62191473184000046, 4.312542294520999242, -317.5000000000030127 ) ) ;
#2501 = ORIENTED_EDGE ( 'NONE', *, *, #3654, .F. ) ;
#2502 = CARTESIAN_POINT ( 'NONE',  ( 11.75341581114999023, -10.21170493764999598, -302.9207377450070453 ) ) ;
#2503 = CARTESIAN_POINT ( 'NONE',  ( 18.90091799877999179, -0.2928069713013998765, -317.4928077629770087 ) ) ;
#2504 = ADVANCED_FACE ( 'NONE', ( #4841 ), #2259, .T. ) ;
#2505 = DIRECTION ( 'NONE',  ( 0.8820010751365653379, 0.000000000000000000, 0.4712473909295871732 ) ) ;
#2506 = PRESENTATION_LAYER_ASSIGNMENT (  '', '', ( #1127 ) ) ;
#2507 = CARTESIAN_POINT ( 'NONE',  ( 10.53744240725999681, 10.62869657088999986, -303.6197174156520759 ) ) ;
#2508 = CARTESIAN_POINT ( 'NONE',  ( -10.25126261553517537, 10.00000004282989785, 314.9999999999999432 ) ) ;
#2509 = VERTEX_POINT ( 'NONE', #10584 ) ;
#2510 = CARTESIAN_POINT ( 'NONE',  ( -17.56330558013000243, -0.6698376231023999150, -314.4150829855000211 ) ) ;
#2511 = DIRECTION ( 'NONE',  ( 0.000000000000000000, 1.000000000000000000, -0.000000000000000000 ) ) ;
#2512 = ORIENTED_EDGE ( 'NONE', *, *, #2068, .T. ) ;
#2513 = CARTESIAN_POINT ( 'NONE',  ( -18.77789454208001985, -4.479159834667000517, 190.4207385301700128 ) ) ;
#2514 = FACE_OUTER_BOUND ( 'NONE', #4926, .T. ) ;
#2515 = CARTESIAN_POINT ( 'NONE',  ( 16.99996037728000076, -1.352915083302999933E-09, -314.9999801883000146 ) ) ;
#2516 = CARTESIAN_POINT ( 'NONE',  ( 10.00000000000000000, 2.500000000000000000, -317.5000000000000000 ) ) ;
#2517 = ORIENTED_EDGE ( 'NONE', *, *, #2809, .T. ) ;
#2518 = CARTESIAN_POINT ( 'NONE',  ( 17.18263598829999950, -2.199757124398999952, 314.4150829855000211 ) ) ;
#2519 = DIRECTION ( 'NONE',  ( 0.7784864941890657919, 0.000000000000000000, 0.6276613564377031551 ) ) ;
#2520 = CARTESIAN_POINT ( 'NONE',  ( 18.44593188493998426, -2.441603908132000011, 319.9928079742500131 ) ) ;
#2521 = CARTESIAN_POINT ( 'NONE',  ( -16.99398431597748171, 6.605820200493087491, 319.0000000000005116 ) ) ;
#2522 = PRODUCT_DEFINITION ( 'UNKNOWN', '', #9717, #10012 ) ;
#2523 = CARTESIAN_POINT ( 'NONE',  ( 17.11849373668000140, 0.6181952683021000317, 314.8616023057000461 ) ) ;
#2524 = ORIENTED_EDGE ( 'NONE', *, *, #3365, .T. ) ;
#2525 = CARTESIAN_POINT ( 'NONE',  ( 1.249193831065165128, -12.49557363514548314, 190.9999999999995737 ) ) ;
#2526 = EDGE_LOOP ( 'NONE', ( #7414, #638, #1615, #1103 ) ) ;
#2527 = ORIENTED_EDGE ( 'NONE', *, *, #6205, .T. ) ;
#2528 = CARTESIAN_POINT ( 'NONE',  ( -2.038789940206844342, -2.521785824191000280, -434.7311834052255790 ) ) ;
#2529 = CARTESIAN_POINT ( 'NONE',  ( 14.21175436428723771, 5.188485551603381651, 315.0000000000000000 ) ) ;
#2530 = CARTESIAN_POINT ( 'NONE',  ( -15.00000000000000000, -0.4945770392355999800, -285.0000000000000000 ) ) ;
#2531 = ORIENTED_EDGE ( 'NONE', *, *, #4895, .T. ) ;
#2532 = CARTESIAN_POINT ( 'NONE',  ( -1.743229001746446682, -2.568129413088056978, -434.7271494043006896 ) ) ;
#2533 = ADVANCED_FACE ( 'NONE', ( #653 ), #3598, .T. ) ;
#2534 = DIRECTION ( 'NONE',  ( 0.000000000000000000, -1.000000000000000000, 0.000000000000000000 ) ) ;
#2535 = CARTESIAN_POINT ( 'NONE',  ( 16.84157450053000105, 5.300668178571999789, 190.0000000000000000 ) ) ;
#2536 = CARTESIAN_POINT ( 'NONE',  ( -14.96226901326146042, -6.078566365972378982, -438.5174415475119076 ) ) ;
#2537 = CARTESIAN_POINT ( 'NONE',  ( -0.5141583095772008782, -2.456010981267997551, -434.7739004999450003 ) ) ;
#2538 = DIRECTION ( 'NONE',  ( 0.000000000000000000, 1.000000000000000000, -0.000000000000000000 ) ) ;
#2539 = AXIS2_PLACEMENT_3D ( 'NONE', #5858, #3560, #1734 ) ;
#2540 = CARTESIAN_POINT ( 'NONE',  ( 11.69962851017000283, 10.23591410519999201, -317.0792622552969533 ) ) ;
#2541 = CARTESIAN_POINT ( 'NONE',  ( 8.369319885711609786, -4.247274070869474727, -525.7071792109185253 ) ) ;
#2542 = EDGE_CURVE ( 'NONE', #4674, #344, #480, .T. ) ;
#2543 = CARTESIAN_POINT ( 'NONE',  ( -1.730441907225505727, -7.305146192242999881, -435.0908526137575905 ) ) ;
#2544 = AXIS2_PLACEMENT_3D ( 'NONE', #6737, #6079, #4316 ) ;
#2545 = DIRECTION ( 'NONE',  ( -0.9942380540931650135, 0.000000000000000000, -0.1071946444232960011 ) ) ;
#2546 = CARTESIAN_POINT ( 'NONE',  ( -1.962614641415807659, -9.435987819058212267, -315.0000000000000000 ) ) ;
#2547 = ORIENTED_EDGE ( 'NONE', *, *, #2556, .T. ) ;
#2548 = CARTESIAN_POINT ( 'NONE',  ( 13.85286411329786560, -6.044949306166734537, -314.5816605312646175 ) ) ;
#2549 = ORIENTED_EDGE ( 'NONE', *, *, #172, .T. ) ;
#2550 = CYLINDRICAL_SURFACE ( 'NONE', #7930, 10.00000000000001599 ) ;
#2551 = ORIENTED_EDGE ( 'NONE', *, *, #9062, .T. ) ;
#2552 = CARTESIAN_POINT ( 'NONE',  ( 20.06707331603001521, 0.4205479510244998220, -302.9207377450070453 ) ) ;
#2553 = CARTESIAN_POINT ( 'NONE',  ( -4.800908653447998553, -11.01413625319999845, -317.4928077629770087 ) ) ;
#2554 = CARTESIAN_POINT ( 'NONE',  ( -19.99999035944999903, 7.277427703818000446E-10, -303.5000000000000000 ) ) ;
#2555 = CARTESIAN_POINT ( 'NONE',  ( -9.379641673262440804, -6.977332597345990095, -437.0255175026235293 ) ) ;
#2556 = EDGE_CURVE ( 'NONE', #9461, #6326, #6334, .T. ) ;
#2557 = CARTESIAN_POINT ( 'NONE',  ( -16.56522182708686941, -3.263825229738949840, 314.4999489731223434 ) ) ;
#2558 = ORIENTED_EDGE ( 'NONE', *, *, #4956, .F. ) ;
#2559 = CARTESIAN_POINT ( 'NONE',  ( -0.6233307549567066452, -7.499999885133000532, -434.1629327817910280 ) ) ;
#2560 = CARTESIAN_POINT ( 'NONE',  ( -3.370560865743999823, 11.33032003377000052, -302.5000000000000000 ) ) ;
#2561 = ORIENTED_EDGE ( 'NONE', *, *, #1869, .F. ) ;
#2562 = CARTESIAN_POINT ( 'NONE',  ( -2.655864369898997435, -12.48600887025999029, 190.4207385301700128 ) ) ;
#2563 = DIRECTION ( 'NONE',  ( 0.000000000000000000, -1.000000000000000000, 0.000000000000000000 ) ) ;
#2564 = CARTESIAN_POINT ( 'NONE',  ( -37.82921798586438911, -9.500000000000001776, -422.3602549205895684 ) ) ;
#2565 = DIRECTION ( 'NONE',  ( 0.000000000000000000, -1.000000000000000000, 0.000000000000000000 ) ) ;
#2566 = CARTESIAN_POINT ( 'NONE',  ( -13.10162021654998732, 9.446493979990000511, 191.1197171614399792 ) ) ;
#2567 = VECTOR ( 'NONE', #5886, 1000.000000000000000 ) ;
#2568 = CIRCLE ( 'NONE', #1184, 3.500000000000006217 ) ;
#2569 = CARTESIAN_POINT ( 'NONE',  ( 15.43693218238999876, -4.538485726840999490, 314.6383426456000052 ) ) ;
#2570 = FACE_OUTER_BOUND ( 'NONE', #1525, .T. ) ;
#2571 = CARTESIAN_POINT ( 'NONE',  ( -19.11656497511998154, -2.646905232783001605, 320.0770942683900557 ) ) ;
#2572 = DIRECTION ( 'NONE',  ( -0.9902680687415800209, 0.000000000000000000, -0.1391731009599967983 ) ) ;
#2573 = CARTESIAN_POINT ( 'NONE',  ( -43.65370867118748777, -7.500000000000000000, -412.6743931307942717 ) ) ;
#2574 = CARTESIAN_POINT ( 'NONE',  ( 6.419414596134000561, 9.427679607337001499, 314.4150829855000211 ) ) ;
#2575 = ADVANCED_FACE ( 'NONE', ( #9730, #3928, #7207, #6557 ), #1619, .F. ) ;
#2576 = ORIENTED_EDGE ( 'NONE', *, *, #6072, .T. ) ;
#2577 = CARTESIAN_POINT ( 'NONE',  ( -7.561138155138405814, -11.58431960382585402, 190.9999999999995737 ) ) ;
#2578 = VERTEX_POINT ( 'NONE', #9303 ) ;
#2579 = VERTEX_POINT ( 'NONE', #6615 ) ;
#2580 = VECTOR ( 'NONE', #5428, 1000.000000000000000 ) ;
#2581 =( BOUNDED_CURVE ( )  B_SPLINE_CURVE ( 3, ( #7578, #9947, #2532, #7421, #170, #5965, #6014, #8332, #9091, #1072, #2642, #3447, #10002, #4358, #119, #1780, #1728, #276, #8222 ),
 .UNSPECIFIED., .F., .T. ) 
 B_SPLINE_CURVE_WITH_KNOTS ( ( 4, 1, 1, 1, 1, 1, 1, 1, 1, 1, 1, 1, 1, 1, 1, 1, 4 ),
 ( 0.000000000000000000, 0.02240047936246757077, 0.1327950495784611662, 0.2340085511830341525, 0.3267384236920149454, 0.4118026492331378074, 0.4900892306436237522, 0.5625168287438816472, 0.6299155825606346237, 0.6928641569844152803, 0.7516748739333113383, 0.8063000023450603848, 0.8556381163399817691, 0.8990751865928527931, 0.9381911258101325313, 0.9762570717716427815, 1.000000000000000000 ),
 .UNSPECIFIED. ) 
 CURVE ( )  GEOMETRIC_REPRESENTATION_ITEM ( )  RATIONAL_B_SPLINE_CURVE ( ( 1.017164269003578481, 1.017164269003578481, 1.017164269003578481, 1.017164269003578481, 1.017164269003578481, 1.017164269003578481, 1.017164269003578481, 1.017164269003578481, 1.017164269003578481, 1.017164269003578481, 1.017164269003578481, 1.017164269003578481, 1.017164269003578481, 1.017164269003578481, 1.017164269003578481, 1.017164269003578481, 1.017164269003578481, 1.017164269003578481, 1.017164269003578481 ) ) 
 REPRESENTATION_ITEM ( '' )  );
#2582 = CARTESIAN_POINT ( 'NONE',  ( -1.093371887104504614, -1.934387371788998111, -435.9299591300448924 ) ) ;
#2583 = MECHANICAL_DESIGN_GEOMETRIC_PRESENTATION_REPRESENTATION (  '', ( #3090 ), #10466 ) ;
#2584 = CARTESIAN_POINT ( 'NONE',  ( 3.689342025446077589, 9.275861061134104801, 315.0000000000001137 ) ) ;
#2585 = ITEM_DEFINED_TRANSFORMATION ( 'NONE', 'NONE', #9210,  #2817 ) ;
#2586 = DIRECTION ( 'NONE',  ( -0.2951854283188012906, 0.000000000000000000, 0.9554399839384188908 ) ) ;
#2587 = ORIENTED_EDGE ( 'NONE', *, *, #3654, .T. ) ;
#2588 = DIRECTION ( 'NONE',  ( -0.4712473909295827323, 0.000000000000000000, 0.8820010751365675583 ) ) ;
#2589 = DIRECTION ( 'NONE',  ( 1.000000000000000000, 0.000000000000000000, 0.000000000000000000 ) ) ;
#2590 = EDGE_CURVE ( 'NONE', #8773, #8790, #6665, .T. ) ;
#2591 = CARTESIAN_POINT ( 'NONE',  ( 14.94331899262999919, 7.078020551493000134, 190.0000000000000000 ) ) ;
#2592 = CARTESIAN_POINT ( 'NONE',  ( 9.994973107563785319, -8.217268576751703080, 314.4999428952268659 ) ) ;
#2593 = CARTESIAN_POINT ( 'NONE',  ( -13.57573464316000056, 3.225916527208000151, -284.9999999999999432 ) ) ;
#2594 = DIRECTION ( 'NONE',  ( 0.3420201433256988555, 0.000000000000000000, -0.9396926207858975477 ) ) ;
#2595 = CARTESIAN_POINT ( 'NONE',  ( 12.84330733966000437, 9.683159015349998455, -317.0792622552969533 ) ) ;
#2596 = EDGE_CURVE ( 'NONE', #9045, #4799, #1833, .T. ) ;
#2597 = CARTESIAN_POINT ( 'NONE',  ( 7.733184489064065303, -4.330975896438657102, -525.7488827635337429 ) ) ;
#2598 = ADVANCED_FACE ( 'NONE', ( #1775 ), #6545, .F. ) ;
#2599 = CARTESIAN_POINT ( 'NONE',  ( -77.67426137820133647, -7.500000000000000000, -345.8174414091573681 ) ) ;
#2600 = PRODUCT_DEFINITION_CONTEXT ( 'detailed design', #303, 'design' ) ;
#2601 = CARTESIAN_POINT ( 'NONE',  ( -12.99025672594594027, -3.249999999996000088, -438.9652310147267826 ) ) ;
#2602 = CARTESIAN_POINT ( 'NONE',  ( 11.93419529315104732, -6.745200168737855329, -315.0000000000000568 ) ) ;
#2603 = VERTEX_POINT ( 'NONE', #6720 ) ;
#2604 = CARTESIAN_POINT ( 'NONE',  ( -17.50000000000126832, 0.7437989020612977287, -314.4963898845654171 ) ) ;
#2605 = VERTEX_POINT ( 'NONE', #7416 ) ;
#2606 = FACE_OUTER_BOUND ( 'NONE', #2310, .T. ) ;
#2607 = VERTEX_POINT ( 'NONE', #58 ) ;
#2608 = CARTESIAN_POINT ( 'NONE',  ( -3.692777996438003196, -12.29248881612998190, -303.6197174156509391 ) ) ;
#2609 = CARTESIAN_POINT ( 'NONE',  ( -18.77313104639999253, -1.494918992088000831, -317.4928077629770087 ) ) ;
#2610 = EDGE_CURVE ( 'NONE', #5924, #4480, #1162, .T. ) ;
#2611 = CARTESIAN_POINT ( 'NONE',  ( -16.21525914616999842, 2.693567875512000054, -315.0848619657999734 ) ) ;
#2612 = CARTESIAN_POINT ( 'NONE',  ( 0.000000000000000000, 0.000000000000000000, 0.000000000000000000 ) ) ;
#2613 = CARTESIAN_POINT ( 'NONE',  ( -20.06707331603001521, -0.4205479510244998220, -302.9207377450070453 ) ) ;
#2614 = CARTESIAN_POINT ( 'NONE',  ( -56.92031869107000119, 2.500000000000000000, -403.1217184488000385 ) ) ;
#2615 = ORIENTED_EDGE ( 'NONE', *, *, #4909, .T. ) ;
#2616 = CARTESIAN_POINT ( 'NONE',  ( -17.16710485141000220, -2.239552065056999997, -314.4150829855000211 ) ) ;
#2617 = CARTESIAN_POINT ( 'NONE',  ( -18.86992372454000133, 1.611776198549999872, -302.4999999999529905 ) ) ;
#2618 = VERTEX_POINT ( 'NONE', #6777 ) ;
#2619 = CIRCLE ( 'NONE', #6036, 20.00000000000000355 ) ;
#2620 = CARTESIAN_POINT ( 'NONE',  ( 19.56918397773000962, -2.861069655901001152, 190.4207385301700128 ) ) ;
#2621 = CARTESIAN_POINT ( 'NONE',  ( 12.98706127646999953, -6.788989183774999603, -315.0000000000001137 ) ) ;
#2622 = CARTESIAN_POINT ( 'NONE',  ( 13.82248977823974734, 5.505663031471445201, -315.0000000000000000 ) ) ;
#2623 = DIRECTION ( 'NONE',  ( 0.9902680687415800209, 0.000000000000000000, 0.1391731009599966873 ) ) ;
#2624 = CARTESIAN_POINT ( 'NONE',  ( 0.7125182177438000863, 12.50545814267000644, 191.1197171614399792 ) ) ;
#2625 = CARTESIAN_POINT ( 'NONE',  ( 10.40890489166000066, -7.434429060800999522, 315.0848619657999734 ) ) ;
#2626 = SURFACE_STYLE_USAGE ( .BOTH. , #1978 ) ;
#2627 = CARTESIAN_POINT ( 'NONE',  ( -51.72607275331812104, -8.000000000000000000, -370.6966883942067739 ) ) ;
#2628 = AXIS2_PLACEMENT_3D ( 'NONE', #7742, #6231, #386 ) ;
#2629 = CARTESIAN_POINT ( 'NONE',  ( 0.6255878334489998194, -12.09339422449000168, 320.0770942683900557 ) ) ;
#2630 = CARTESIAN_POINT ( 'NONE',  ( -17.44869542604064705, 0.8969788624277408307, 314.4999390965243720 ) ) ;
#2631 = CARTESIAN_POINT ( 'NONE',  ( 19.86375996897344720, 1.775925728142829341, -303.4999999999999432 ) ) ;
#2632 = CARTESIAN_POINT ( 'NONE',  ( 10.50000150490000017, 7.882579085736000302, 314.6383426456000052 ) ) ;
#2633 = ORIENTED_EDGE ( 'NONE', *, *, #1410, .T. ) ;
#2634 = CARTESIAN_POINT ( 'NONE',  ( -2.000000000000000000, 2.500000000000000000, -409.5000000000000000 ) ) ;
#2635 = CARTESIAN_POINT ( 'NONE',  ( 13.15302580975001234, 9.418553998452996012, 318.8802828394900644 ) ) ;
#2636 = ORIENTED_EDGE ( 'NONE', *, *, #3707, .T. ) ;
#2637 = CARTESIAN_POINT ( 'NONE',  ( -7.895874901503558085, -3.499933318827000317, -436.7910735983360269 ) ) ;
#2638 = CARTESIAN_POINT ( 'NONE',  ( -0.9841565935054803482, 9.488387273935385835, 314.9999999999999432 ) ) ;
#2639 = ITEM_DEFINED_TRANSFORMATION ( 'NONE', 'NONE', #5073,  #2817 ) ;
#2640 = CARTESIAN_POINT ( 'NONE',  ( -15.00000000000325784, 8.632726818195413123E-17, -284.9999999999999432 ) ) ;
#2641 = ORIENTED_EDGE ( 'NONE', *, *, #10218, .T. ) ;
#2642 = CARTESIAN_POINT ( 'NONE',  ( -0.9130074951844157072, -2.517145578169100339, -434.3665436561622641 ) ) ;
#2643 = PRESENTATION_STYLE_ASSIGNMENT (( #6621 ) ) ;
#2644 = VECTOR ( 'NONE', #4287, 1000.000000000000000 ) ;
#2645 = CARTESIAN_POINT ( 'NONE',  ( -1.290325097615000027, 11.49300988401000012, 190.0000000000000000 ) ) ;
#2646 = CARTESIAN_POINT ( 'NONE',  ( -51.41224207513210587, -8.000000000000000000, -371.0859316413305464 ) ) ;
#2647 = CARTESIAN_POINT ( 'NONE',  ( 15.00000000000325784, -8.632726818195413123E-17, -284.9999999999999432 ) ) ;
#2648 = ORIENTED_EDGE ( 'NONE', *, *, #899, .T. ) ;
#2649 = CARTESIAN_POINT ( 'NONE',  ( -0.3764627761248945381, -8.000000000000000000, -361.1540620660322816 ) ) ;
#2650 = AXIS2_PLACEMENT_3D ( 'NONE', #2199, #3708, #8535 ) ;
#2651 = FACE_OUTER_BOUND ( 'NONE', #1528, .T. ) ;
#2652 = CARTESIAN_POINT ( 'NONE',  ( -1.630004931178638428, -7.334531690290998718, -435.2814510150427054 ) ) ;
#2653 = CARTESIAN_POINT ( 'NONE',  ( 17.19853431800999743, 2.231396706187000145, -315.0000000000000000 ) ) ;
#2654 = CIRCLE ( 'NONE', #5903, 0.5000000000000079936 ) ;
#2655 = CARTESIAN_POINT ( 'NONE',  ( 9.619051408962835836, -7.822710805390641120, -315.0000000000000568 ) ) ;
#2656 = ORIENTED_EDGE ( 'NONE', *, *, #4640, .F. ) ;
#2657 = FACE_OUTER_BOUND ( 'NONE', #6360, .T. ) ;
#2658 = CARTESIAN_POINT ( 'NONE',  ( -19.99984272814741715, -0.5882336804855470280, -316.5000000000004547 ) ) ;
#2659 = ORIENTED_EDGE ( 'NONE', *, *, #6694, .F. ) ;
#2660 = CARTESIAN_POINT ( 'NONE',  ( -14.74684780783305449, -5.500000000000000000, -439.3959507452315165 ) ) ;
#2661 = EDGE_LOOP ( 'NONE', ( #3907, #10072, #9299, #3463 ) ) ;
#2662 = MECHANICAL_DESIGN_GEOMETRIC_PRESENTATION_REPRESENTATION (  '', ( #421 ), #4379 ) ;
#2663 = CARTESIAN_POINT ( 'NONE',  ( 1.546121016139999638, 11.35842264293001591, -317.4928077629770087 ) ) ;
#2664 = AXIS2_PLACEMENT_3D ( 'NONE', #4597, #4651, #7922 ) ;
#2665 = CARTESIAN_POINT ( 'NONE',  ( -16.86005112630999037, -5.110605191077000065, -317.4928077629770087 ) ) ;
#2666 = CARTESIAN_POINT ( 'NONE',  ( -41.41721991556968874, -8.000000000000000000, -366.3159076589344636 ) ) ;
#2667 = VECTOR ( 'NONE', #10082, 1000.000000000000000 ) ;
#2668 =( NAMED_UNIT ( * ) SI_UNIT ( $, .STERADIAN. ) SOLID_ANGLE_UNIT ( ) );
#2669 = VECTOR ( 'NONE', #5090, 1000.000000000000000 ) ;
#2670 = CARTESIAN_POINT ( 'NONE',  ( 19.98381222165001248, -0.4032365313531999784, -303.6197174156509391 ) ) ;
#2671 = ORIENTED_EDGE ( 'NONE', *, *, #9703, .T. ) ;
#2672 = CARTESIAN_POINT ( 'NONE',  ( -2.000000000000000000, -9.500000000000000000, -406.0000000000000000 ) ) ;
#2673 = EDGE_CURVE ( 'NONE', #9383, #563, #6489, .T. ) ;
#2674 = CARTESIAN_POINT ( 'NONE',  ( -10.14429053679999981, 9.716529139337000132, -302.5000000000000000 ) ) ;
#2675 = VERTEX_POINT ( 'NONE', #9253 ) ;
#2676 = CARTESIAN_POINT ( 'NONE',  ( 16.34052447997000357, -7.211013068275999416, 191.1197171614399792 ) ) ;
#2677 = CARTESIAN_POINT ( 'NONE',  ( -15.67978886374999803, -4.575336738469999887, -314.4944826805095772 ) ) ;
#2678 = CARTESIAN_POINT ( 'NONE',  ( 15.43598538069025139, 3.955158390306824590, -315.0000000000000568 ) ) ;
#2679 = EDGE_CURVE ( 'NONE', #9887, #7283, #8427, .T. ) ;
#2680 = CARTESIAN_POINT ( 'NONE',  ( -19.95847042008000827, 0.9399586737018998939, 191.1197171614399792 ) ) ;
#2681 = CARTESIAN_POINT ( 'NONE',  ( 12.07130791616000032, -6.858215270785999351, 314.8616023057000461 ) ) ;
#2682 =( NAMED_UNIT ( * ) SI_UNIT ( $, .STERADIAN. ) SOLID_ANGLE_UNIT ( ) );
#2683 = EDGE_CURVE ( 'NONE', #5580, #4923, #1123, .T. ) ;
#2684 = CARTESIAN_POINT ( 'NONE',  ( -5.416173751597343156, -12.50000000000000000, -337.7825848737071510 ) ) ;
#2685 = CARTESIAN_POINT ( 'NONE',  ( 18.12318599310000167, -3.186119256560000945, 319.9928079742500131 ) ) ;
#2686 = LINE ( 'NONE', #5037, #10175 ) ;
#2687 = CARTESIAN_POINT ( 'NONE',  ( 1.984036549750167300, 12.45525792938212639, -303.4999999999990905 ) ) ;
#2688 = CARTESIAN_POINT ( 'NONE',  ( 12.21495827233999876, 7.290170534263999969, 314.4150829855000211 ) ) ;
#2689 = ORIENTED_EDGE ( 'NONE', *, *, #2987, .T. ) ;
#2690 = CARTESIAN_POINT ( 'NONE',  ( 17.01113700077726776, -6.587853872568209646, 190.9999999999995737 ) ) ;
#2691 = CARTESIAN_POINT ( 'NONE',  ( 9.099181536070998888, 11.22222323403999766, 319.5792614743400009 ) ) ;
#2692 = CARTESIAN_POINT ( 'NONE',  ( 18.99999441908000009, 1.671652446847999990E-07, 319.0000000000000000 ) ) ;
#2693 = CARTESIAN_POINT ( 'NONE',  ( 4.780298404687055580, 9.113031460416761931, 315.0000000000000000 ) ) ;
#2694 = LINE ( 'NONE', #6012, #1549 ) ;
#2695 = EDGE_LOOP ( 'NONE', ( #10232, #9170, #8030, #5805 ) ) ;
#2696 = CARTESIAN_POINT ( 'NONE',  ( -2.000000000003786749, -8.000000000000000000, -409.4999999999758415 ) ) ;
#2697 = AXIS2_PLACEMENT_3D ( 'NONE', #6841, #10009, #5264 ) ;
#2698 = EDGE_CURVE ( 'NONE', #8515, #2607, #8883, .T. ) ;
#2699 = CARTESIAN_POINT ( 'NONE',  ( -3.339933055294988851, -9.000000000000001776, -397.0720243238112630 ) ) ;
#2700 = CARTESIAN_POINT ( 'NONE',  ( -15.24002748250033967, 4.193218933356376965, -315.0000000000000000 ) ) ;
#2701 = CARTESIAN_POINT ( 'NONE',  ( -43.33032886862778099, -8.000000000000000000, -402.2979831847262631 ) ) ;
#2702 = CARTESIAN_POINT ( 'NONE',  ( -19.08872200864999868, -7.500000000000000000, -429.3350920981999934 ) ) ;
#2703 = DIRECTION ( 'NONE',  ( -0.6333991923391583123, 0.000000000000000000, 0.7738252148541697739 ) ) ;
#2704 = CARTESIAN_POINT ( 'NONE',  ( -78.61675616006050404, -2.500000000000000000, -344.0534392588842252 ) ) ;
#2705 = UNCERTAINTY_MEASURE_WITH_UNIT (LENGTH_MEASURE( 1.000000000000000082E-05 ), #4488, 'distance_accuracy_value', 'NONE');
#2706 = LINE ( 'NONE', #4318, #5817 ) ;
#2707 = ORIENTED_EDGE ( 'NONE', *, *, #6734, .F. ) ;
#2708 = AXIS2_PLACEMENT_3D ( 'NONE', #8060, #2476, #9030 ) ;
#2709 = DIRECTION ( 'NONE',  ( 0.03413883980201725538, 0.000000000000000000, -0.9994170999222358187 ) ) ;
#2710 = CARTESIAN_POINT ( 'NONE',  ( 16.88284456999480554, -6.727435487264400216, -316.5000000000004547 ) ) ;
#2711 = ORIENTED_EDGE ( 'NONE', *, *, #6008, .F. ) ;
#2712 = EDGE_CURVE ( 'NONE', #9606, #7707, #9555, .T. ) ;
#2713 = FACE_OUTER_BOUND ( 'NONE', #6800, .T. ) ;
#2714 = ORIENTED_EDGE ( 'NONE', *, *, #235, .T. ) ;
#2715 = CARTESIAN_POINT ( 'NONE',  ( -18.78102408959999536, 1.459157757289999413, -317.4928077629770087 ) ) ;
#2716 = CARTESIAN_POINT ( 'NONE',  ( -18.28030995243001655, -2.924502517761999876, -317.4928077629770087 ) ) ;
#2717 = CARTESIAN_POINT ( 'NONE',  ( -1.873948611771682149, -7.500000000000000888, -349.2478646809681777 ) ) ;
#2718 = CARTESIAN_POINT ( 'NONE',  ( -10.51805095810000346, 10.63699911018001210, -303.6197174156520759 ) ) ;
#2719 = PLANE ( 'NONE',  #9604 ) ;
#2720 = VERTEX_POINT ( 'NONE', #1329 ) ;
#2721 = CARTESIAN_POINT ( 'NONE',  ( 19.00000000000000000, 0.000000000000000000, 190.0000000000100044 ) ) ;
#2722 = DIRECTION ( 'NONE',  ( 0.000000000000000000, 1.000000000000000000, 0.000000000000000000 ) ) ;
#2723 = EDGE_CURVE ( 'NONE', #2579, #1205, #3601, .T. ) ;
#2724 = ORIENTED_EDGE ( 'NONE', *, *, #3777, .T. ) ;
#2725 = CARTESIAN_POINT ( 'NONE',  ( 7.995233561666595712, -7.656480000000000175, -523.7425978728656446 ) ) ;
#2726 = DIRECTION ( 'NONE',  ( -0.1071946444232964035, 0.000000000000000000, 0.9942380540931649024 ) ) ;
#2727 = CARTESIAN_POINT ( 'NONE',  ( 18.78105930652002087, -1.458809753444000767, -302.5071922382879279 ) ) ;
#2728 = CARTESIAN_POINT ( 'NONE',  ( 11.06049270995999123, 10.50744457173999713, 190.4207385301700128 ) ) ;
#2729 = EDGE_CURVE ( 'NONE', #5743, #4172, #6115, .T. ) ;
#2730 = CARTESIAN_POINT ( 'NONE',  ( -1.867120547373915418, -7.452566320787000542, -434.7177009740820495 ) ) ;
#2731 = EDGE_CURVE ( 'NONE', #8080, #700, #1167, .T. ) ;
#2732 = DIRECTION ( 'NONE',  ( 0.6276613564376841703, 0.000000000000000000, -0.7784864941890811130 ) ) ;
#2733 = CARTESIAN_POINT ( 'NONE',  ( -10.21681110195000031, -10.83745499882999574, 319.5792614743400009 ) ) ;
#2734 = CARTESIAN_POINT ( 'NONE',  ( -17.05540562798465842, 2.295823712133366445, 314.4999398562647457 ) ) ;
#2735 = CARTESIAN_POINT ( 'NONE',  ( -17.49999998521812117, 5.867334131620513205, 189.9999999999998010 ) ) ;
#2736 = CARTESIAN_POINT ( 'NONE',  ( 17.36972170382999892, 0.04551883977364000466, 314.6383426456000052 ) ) ;
#2737 = EDGE_LOOP ( 'NONE', ( #9055, #9053, #1639, #5609, #7501 ) ) ;
#2738 = CARTESIAN_POINT ( 'NONE',  ( 11.17208682466014302, -10.37722895585535454, 190.9999999999995737 ) ) ;
#2739 = CARTESIAN_POINT ( 'NONE',  ( -8.796035389134001292, 11.31703133948999707, 319.5792614743400009 ) ) ;
#2740 = CIRCLE ( 'NONE', #1356, 12.49999999999998934 ) ;
#2741 = CIRCLE ( 'NONE', #4112, 12.99999999999997868 ) ;
#2742 = CARTESIAN_POINT ( 'NONE',  ( -1.119552414421413511, -2.606163259540000610, -435.7158780125686235 ) ) ;
#2743 = CARTESIAN_POINT ( 'NONE',  ( -5.334308159457383347, 9.025045582129868293, 314.9999999999999432 ) ) ;
#2744 = DIRECTION ( 'NONE',  ( -0.6697079934638360266, 0.000000000000000000, -0.7426245373610022016 ) ) ;
#2745 = AXIS2_PLACEMENT_3D ( 'NONE', #2601, #7695, #3405 ) ;
#2746 = CARTESIAN_POINT ( 'NONE',  ( 15.28688047792000049, -6.812924772642000804, -302.5000000000000000 ) ) ;
#2747 = CARTESIAN_POINT ( 'NONE',  ( -37.57635160138833896, -7.500000000000000888, -403.2777420460153053 ) ) ;
#2748 = CARTESIAN_POINT ( 'NONE',  ( 18.78940217795999956, 1.754852253524999961, 190.0000000000000000 ) ) ;
#2749 = CARTESIAN_POINT ( 'NONE',  ( 5.453155204153861568, -9.512440879258083015, 314.4999437815906163 ) ) ;
#2750 = CARTESIAN_POINT ( 'NONE',  ( 18.89053622393001675, 0.06335528492990002980, 190.0071920248299477 ) ) ;
#2751 = CARTESIAN_POINT ( 'NONE',  ( -5.416173639476232538, -7.500000000000000888, -337.7825852366146364 ) ) ;
#2752 = CARTESIAN_POINT ( 'NONE',  ( 6.685859146470366277, -4.450907801408272135, -525.2546656924790796 ) ) ;
#2753 = CARTESIAN_POINT ( 'NONE',  ( 7.584651611965206541, -5.651391369166294254, -525.7002755026068144 ) ) ;
#2754 = DIRECTION ( 'NONE',  ( 0.000000000000000000, 0.000000000000000000, -1.000000000000000000 ) ) ;
#2755 = ORIENTED_EDGE ( 'NONE', *, *, #8377, .T. ) ;
#2756 = CARTESIAN_POINT ( 'NONE',  ( 8.736690731312993563, 10.08117623986000133, 319.9928079742500131 ) ) ;
#2757 = CIRCLE ( 'NONE', #6859, 999.9999999999997726 ) ;
#2758 = CARTESIAN_POINT ( 'NONE',  ( -33.34106825788445150, -2.500000000000000000, -439.6766126514281154 ) ) ;
#2759 = DIRECTION ( 'NONE',  ( -0.9554399839384176696, 0.000000000000000000, -0.2951854283188049544 ) ) ;
#2760 = ORIENTED_EDGE ( 'NONE', *, *, #5354, .T. ) ;
#2761 = APPLICATION_CONTEXT ( 'automotive_design' ) ;
#2762 = AXIS2_PLACEMENT_3D ( 'NONE', #9901, #4149, #8225 ) ;
#2763 = DIRECTION ( 'NONE',  ( -3.267118270366935116E-06, -8.358028872200239840E-13, -0.9999999999946629359 ) ) ;
#2764 = CARTESIAN_POINT ( 'NONE',  ( -19.56018598331999314, 0.5259244641825996380, -317.5770954168139610 ) ) ;
#2765 = DIRECTION ( 'NONE',  ( -0.9712267471052594692, 0.000000000000000000, -0.2381566831044984178 ) ) ;
#2766 = CARTESIAN_POINT ( 'NONE',  ( 16.63787452912263731, 3.035984518719835101, -314.5459997954137066 ) ) ;
#2767 = FACE_BOUND ( 'NONE', #4216, .T. ) ;
#2768 = TOROIDAL_SURFACE ( 'NONE', #8769, 15.50000000000000000, 0.5000000000000000000 ) ;
#2769 = VERTEX_POINT ( 'NONE', #4609 ) ;
#2770 = FILL_AREA_STYLE_COLOUR ( '', #5918 ) ;
#2771 = DIRECTION ( 'NONE',  ( -0.9712267471052612455, 0.000000000000000000, -0.2381566831044910626 ) ) ;
#2772 = ORIENTED_EDGE ( 'NONE', *, *, #4735, .T. ) ;
#2773 = CARTESIAN_POINT ( 'NONE',  ( 13.10162021654998732, -9.446493979990000511, 191.1197171614399792 ) ) ;
#2774 = ORIENTED_EDGE ( 'NONE', *, *, #1413, .F. ) ;
#2775 = DIRECTION ( 'NONE',  ( 0.000000000000000000, -1.000000000000000000, 0.000000000000000000 ) ) ;
#2776 = CARTESIAN_POINT ( 'NONE',  ( 0.000000000000000000, 10.00000000000000000, 315.0000000000000000 ) ) ;
#2777 = CARTESIAN_POINT ( 'NONE',  ( -10.12800840543000724, 10.78031690431999756, 191.1197171614399792 ) ) ;
#2778 = ADVANCED_FACE ( 'NONE', ( #10309, #7885 ), #2945, .T. ) ;
#2779 = CARTESIAN_POINT ( 'NONE',  ( -0.5013770514288425906, -7.487604982435999368, -434.1602016854106978 ) ) ;
#2780 = SHAPE_REPRESENTATION_RELATIONSHIP ( 'NONE' , 'NONE' ,  #4085, #5834 ) ;
#2781 = CARTESIAN_POINT ( 'NONE',  ( -72.90663470102438737, -8.000000000000000000, -371.7168990826883714 ) ) ;
#2782 = PRODUCT_DEFINITION_SHAPE ( 'NONE', 'NONE',  #10629 ) ;
#2783 = CARTESIAN_POINT ( 'NONE',  ( -20.06710154196001739, 0.4210530330733002757, 319.5792614743400009 ) ) ;
#2784 = AXIS2_PLACEMENT_3D ( 'NONE', #8277, #1942, #4205 ) ;
#2785 = CARTESIAN_POINT ( 'NONE',  ( -10.00000000000000000, 2.500000000000000000, -317.5000000000000000 ) ) ;
#2786 = CARTESIAN_POINT ( 'NONE',  ( -14.72449281369000040, 5.549439731021000632, 314.4150829855000211 ) ) ;
#2787 = VERTEX_POINT ( 'NONE', #8633 ) ;
#2788 = CARTESIAN_POINT ( 'NONE',  ( -19.99996770037257221, -0.3054858693455834162, 190.9999999999995737 ) ) ;
#2789 = ORIENTED_EDGE ( 'NONE', *, *, #899, .F. ) ;
#2790 = CARTESIAN_POINT ( 'NONE',  ( -20.00506338957998409, 0.1012955751877999966, 318.8802828394900644 ) ) ;
#2791 = EDGE_CURVE ( 'NONE', #3089, #6862, #532, .T. ) ;
#2792 = AXIS2_PLACEMENT_3D ( 'NONE', #4985, #8368, #1058 ) ;
#2793 = CARTESIAN_POINT ( 'NONE',  ( -78.61675616006050404, -2.500000000000000000, -344.0534392588842252 ) ) ;
#2794 = DIRECTION ( 'NONE',  ( 0.2728306852451984343, 0.000000000000000000, 0.9620620651437388204 ) ) ;
#2795 = CARTESIAN_POINT ( 'NONE',  ( -76.33371517498638070, -7.500000000000000000, -329.2281998388791635 ) ) ;
#2796 = CARTESIAN_POINT ( 'NONE',  ( 20.00000000000000000, 0.000000000000000000, 191.0000000000000000 ) ) ;
#2797 = CARTESIAN_POINT ( 'NONE',  ( -26.31853765676889267, -9.633703999999999823, -432.7407288192795249 ) ) ;
#2798 = CARTESIAN_POINT ( 'NONE',  ( 3.875825478601963248, -7.500000000000000000, -431.3627451401119970 ) ) ;
#2799 = ADVANCED_FACE ( 'NONE', ( #6064 ), #7094, .F. ) ;
#2800 = LINE ( 'NONE', #2646, #4618 ) ;
#2801 = AXIS2_PLACEMENT_3D ( 'NONE', #5089, #9131, #1767 ) ;
#2802 = CARTESIAN_POINT ( 'NONE',  ( -1.205561540619000116, 11.37600766585000933, 190.0071920248299477 ) ) ;
#2803 = CARTESIAN_POINT ( 'NONE',  ( -1.873948611771682149, -7.500000000000000888, -349.2478646809681777 ) ) ;
#2804 = B_SPLINE_SURFACE_WITH_KNOTS ( 'NONE', 3, 1, ( 
 ( #10604, #4106 ),
 ( #6743, #3296 ),
 ( #2498, #5812 ),
 ( #1849, #4913 ),
 ( #5010, #827 ),
 ( #4057, #4962 ),
 ( #8288, #928 ),
 ( #5764, #874 ),
 ( #3246, #6524 ),
 ( #7386, #9805 ),
 ( #1688, #3408 ),
 ( #9963, #2604 ),
 ( #5865, #6182 ) ),
 .UNSPECIFIED., .F., .F., .F.,
 ( 4, 1, 1, 1, 1, 1, 1, 1, 1, 1, 4 ),
 ( 2, 2 ),
 ( 0.01923076854978476163, 0.09935897435896999530, 0.1794871794871999993, 0.2596153846154000133, 0.3397435897436000274, 0.5000000000000000000, 0.6602564102564000281, 0.7403846153845999867, 0.8205128205128000562, 0.9006410256410000148, 0.9807692307692000844 ),
 ( 0.000000000000000000, 1.000000000000000000 ),
 .UNSPECIFIED. ) ;
#2805 = CARTESIAN_POINT ( 'NONE',  ( -12.86189863199293093, -5.758762107780500017, -438.9337381413729418 ) ) ;
#2806 = CARTESIAN_POINT ( 'NONE',  ( -1.214899924133375331, -7.403467476614999043, -435.1227120718077686 ) ) ;
#2807 = CARTESIAN_POINT ( 'NONE',  ( 12.16656789651012005, -6.621481216618937182, 314.9999999999999432 ) ) ;
#2808 = CARTESIAN_POINT ( 'NONE',  ( -12.17979804859000126, 7.053762231097000068, -314.6383426456000052 ) ) ;
#2809 = EDGE_CURVE ( 'NONE', #10444, #6682, #5356, .T. ) ;
#2810 = VERTEX_POINT ( 'NONE', #1989 ) ;
#2811 = CARTESIAN_POINT ( 'NONE',  ( -8.447271450478007537, 10.17170359172999738, 319.9928079742500131 ) ) ;
#2812 = LINE ( 'NONE', #392, #3333 ) ;
#2813 = CYLINDRICAL_SURFACE ( 'NONE', #3478, 3.499999999999998668 ) ;
#2814 = ORIENTED_EDGE ( 'NONE', *, *, #3455, .T. ) ;
#2815 = CARTESIAN_POINT ( 'NONE',  ( -18.87178158963000030, -0.3573130366704001526, -317.4928077629770087 ) ) ;
#2816 = CARTESIAN_POINT ( 'NONE',  ( 12.90264537120001798, -9.651629027462002242, -317.0792622552969533 ) ) ;
#2817 = AXIS2_PLACEMENT_3D ( 'NONE', #8634, #3966, #3161 ) ;
#2818 = LINE ( 'NONE', #6093, #4530 ) ;
#2819 = ORIENTED_EDGE ( 'NONE', *, *, #2463, .F. ) ;
#2820 = AXIS2_PLACEMENT_3D ( 'NONE', #2370, #3173, #8866 ) ;
#2821 = CARTESIAN_POINT ( 'NONE',  ( -49.82771619714345235, -2.500000000000000000, -415.9731248673013511 ) ) ;
#2822 = CIRCLE ( 'NONE', #4710, 12.50000000608002715 ) ;
#2824 = VERTEX_POINT ( 'NONE', #4557 ) ;
#2823 = CIRCLE ( 'NONE', #8826, 15.00000000000001776 ) ;
#2825 = CARTESIAN_POINT ( 'NONE',  ( 15.66827725153000017, -6.479182156166999995, 190.0000000000000000 ) ) ;
#2826 = CARTESIAN_POINT ( 'NONE',  ( -59.08872748607741698, -2.500000000000000000, -420.9212224720619702 ) ) ;
#2827 = CONICAL_SURFACE ( 'NONE', #256, 3.400000000000014122, 0.7853981633975631871 ) ;
#2828 = ADVANCED_FACE ( 'NONE', ( #478 ), #6275, .T. ) ;
#2829 = ORIENTED_EDGE ( 'NONE', *, *, #4577, .T. ) ;
#2830 = CARTESIAN_POINT ( 'NONE',  ( -13.01115177740000384, -9.495820311550003723, 191.1197171614399792 ) ) ;
#2831 = ORIENTED_EDGE ( 'NONE', *, *, #8386, .F. ) ;
#2832 = CARTESIAN_POINT ( 'NONE',  ( -16.39045651208371979, -2.501479531468998818, 315.0000000000000000 ) ) ;
#2833 = CYLINDRICAL_SURFACE ( 'NONE', #924, 12.49999999999998757 ) ;
#2834 = CARTESIAN_POINT ( 'NONE',  ( 19.14223954934999483, 3.638712114223002558, 191.1197171614399792 ) ) ;
#2835 = CIRCLE ( 'NONE', #1282, 29.99999999999998224 ) ;
#2836 = CIRCLE ( 'NONE', #8833, 5.000000000000004441 ) ;
#2837 = AXIS2_PLACEMENT_3D ( 'NONE', #8842, #5662, #10447 ) ;
#2838 = CARTESIAN_POINT ( 'NONE',  ( -1.207139762621110890, -7.484635725423999908, -434.4480596911860175 ) ) ;
#2839 = CARTESIAN_POINT ( 'NONE',  ( -19.96334758606998605, -0.8982332345458986511, 318.8802828394900644 ) ) ;
#2840 = CARTESIAN_POINT ( 'NONE',  ( 16.89986669904000394, -0.5583209492923999484, -315.0848619657999734 ) ) ;
#2841 = CARTESIAN_POINT ( 'NONE',  ( -16.55686070535999832, 1.955716293870999767, 315.0848619657999734 ) ) ;
#2842 = ORIENTED_EDGE ( 'NONE', *, *, #5598, .F. ) ;
#2843 = DIRECTION ( 'NONE',  ( 0.000000000000000000, 1.000000000000000000, 0.000000000000000000 ) ) ;
#2844 = CARTESIAN_POINT ( 'NONE',  ( -0.7342372444761647854, -7.494317894969175775, -434.2532513144291215 ) ) ;
#2845 = LINE ( 'NONE', #7139, #3275 ) ;
#2846 = DIRECTION ( 'NONE',  ( 0.000000000000000000, 0.000000000000000000, 1.000000000000000000 ) ) ;
#2847 = CARTESIAN_POINT ( 'NONE',  ( -16.83787941357387297, 1.297844089352232944, 315.0000000000000568 ) ) ;
#2848 = CARTESIAN_POINT ( 'NONE',  ( 11.71572875238734213, -12.50000000010304113, 190.9999999999999432 ) ) ;
#2849 =( GEOMETRIC_REPRESENTATION_CONTEXT ( 3 ) GLOBAL_UNCERTAINTY_ASSIGNED_CONTEXT ( ( #8497 ) ) GLOBAL_UNIT_ASSIGNED_CONTEXT ( ( #4168, #2052, #2668 ) ) REPRESENTATION_CONTEXT ( 'NONE', 'WORKASPACE' ) );
#2850 = CARTESIAN_POINT ( 'NONE',  ( 19.79155829785256415, 1.881978406165077722, 319.0000000000005116 ) ) ;
#2851 = CARTESIAN_POINT ( 'NONE',  ( -17.01838671672000203, -2.500000000000000000, -497.7560445212000104 ) ) ;
#2852 = DIRECTION ( 'NONE',  ( 0.000000000000000000, -1.000000000000000000, 0.000000000000000000 ) ) ;
#2853 = CARTESIAN_POINT ( 'NONE',  ( -75.78927181448300132, -2.500000000000000000, -349.3454457097035970 ) ) ;
#2854 = CARTESIAN_POINT ( 'NONE',  ( -8.021995458420214220, 8.375882622524637000, -315.0000000000000568 ) ) ;
#2855 = CARTESIAN_POINT ( 'NONE',  ( 2.556522775252001445, 11.29259618907000196, 190.0071920248299477 ) ) ;
#2856 = CARTESIAN_POINT ( 'NONE',  ( 3.875825478601963248, -7.656480000000000175, -431.3627451401119970 ) ) ;
#2857 = CARTESIAN_POINT ( 'NONE',  ( 12.36094278317000139, -8.718445687105001340, -317.5000000000000000 ) ) ;
#2858 = FACE_OUTER_BOUND ( 'NONE', #7879, .T. ) ;
#2859 = DIRECTION ( 'NONE',  ( 0.000000000000000000, 0.000000000000000000, 1.000000000000000000 ) ) ;
#2860 = CARTESIAN_POINT ( 'NONE',  ( 11.74237836840727311, -6.849546447955716211, 315.0000000000000000 ) ) ;
#2861 = CARTESIAN_POINT ( 'NONE',  ( -10.67587555525000020, 8.049811041411000900, -314.4150829855000211 ) ) ;
#2862 = ORIENTED_EDGE ( 'NONE', *, *, #9957, .F. ) ;
#2863 = CARTESIAN_POINT ( 'NONE',  ( -17.33328289455318938, -2.867118240563160875E-08, 314.6666162271453118 ) ) ;
#2864 = CARTESIAN_POINT ( 'NONE',  ( -3.357323174585255643, -12.33819210890098894, -316.5000000000004547 ) ) ;
#2865 = DIRECTION ( 'NONE',  ( -0.4712473909295803454, 0.000000000000000000, 0.8820010751365688906 ) ) ;
#2866 = ORIENTED_EDGE ( 'NONE', *, *, #7339, .T. ) ;
#2867 = CARTESIAN_POINT ( 'NONE',  ( -16.88563860788000781, 5.080169144092001154, -317.4928077629770087 ) ) ;
#2868 = CARTESIAN_POINT ( 'NONE',  ( -20.10111883311001080, -0.3733660053931999734, -317.0792622552969533 ) ) ;
#2869 = EDGE_CURVE ( 'NONE', #8301, #4592, #7779, .T. ) ;
#2870 = B_SPLINE_CURVE_WITH_KNOTS ( 'NONE', 3,
 ( #6499, #1614, #4886, #8005, #3057, #1445, #8107, #8165, #591, #10521, #802, #6442, #2308 ),
 .UNSPECIFIED., .F., .F.,
 ( 4, 1, 1, 1, 1, 1, 1, 1, 1, 1, 4 ),
 ( 0.000000000000000000, 0.08333333333333001192, 0.1666666666667000196, 0.2500000000000000000, 0.3333333333333000081, 0.5000000000000000000, 0.6666666666667000474, 0.7500000000000000000, 0.8333333333333000637, 0.9166666666667000474, 1.000000000000000000 ),
 .UNSPECIFIED. ) ;
#2871 = CARTESIAN_POINT ( 'NONE',  ( -28.01838671672000203, -2.500000000000000000, -497.7560445212000104 ) ) ;
#2872 = EDGE_CURVE ( 'NONE', #3553, #344, #4406, .T. ) ;
#2873 = CARTESIAN_POINT ( 'NONE',  ( 3.650011388878862562, 9.782272988550909432, -314.5118284007356237 ) ) ;
#2874 = VERTEX_POINT ( 'NONE', #3748 ) ;
#2875 = CARTESIAN_POINT ( 'NONE',  ( 0.000000000000000000, 0.000000000000000000, -302.5000000000000000 ) ) ;
#2876 = EDGE_LOOP ( 'NONE', ( #10133, #1641, #3155, #9482 ) ) ;
#2877 = DIRECTION ( 'NONE',  ( 0.000000000000000000, -1.000000000000000000, 0.000000000000000000 ) ) ;
#2878 = ORIENTED_EDGE ( 'NONE', *, *, #422, .F. ) ;
#2879 = DIRECTION ( 'NONE',  ( 0.000000000000000000, -1.000000000000000000, 0.000000000000000000 ) ) ;
#2880 = CARTESIAN_POINT ( 'NONE',  ( 1.615578127792000274, -11.35484692374000737, -302.5071922382879279 ) ) ;
#2881 = DIRECTION ( 'NONE',  ( 0.1173809667161562209, 0.000000000000000000, -0.9930869592602555862 ) ) ;
#2882 = AXIS2_PLACEMENT_3D ( 'NONE', #4088, #8114, #9673 ) ;
#2883 = ADVANCED_FACE ( 'NONE', ( #7680 ), #9329, .F. ) ;
#2884 = CARTESIAN_POINT ( 'NONE',  ( -41.41721991556968874, -7.500000000000000888, -366.3159076589344636 ) ) ;
#2885 = CARTESIAN_POINT ( 'NONE',  ( 0.1580967862520001599, 11.39739484195000330, -302.5071922382879279 ) ) ;
#2886 = CARTESIAN_POINT ( 'NONE',  ( 18.24388381812998361, -5.273776366776003144, 319.5792614743400009 ) ) ;
#2887 = CARTESIAN_POINT ( 'NONE',  ( 16.10362618234000109, -3.713712614977999760, -314.6383426456000052 ) ) ;
#2888 = CARTESIAN_POINT ( 'NONE',  ( -16.89986669904000394, 0.5583209492923999484, 315.0848619657999734 ) ) ;
#2889 = EDGE_LOOP ( 'NONE', ( #8940, #2351, #1650, #7221 ) ) ;
#2890 = CARTESIAN_POINT ( 'NONE',  ( -19.14871320452657244, -3.641870911972378444, 190.9999999999995737 ) ) ;
#2891 = ORIENTED_EDGE ( 'NONE', *, *, #543, .F. ) ;
#2892 = CARTESIAN_POINT ( 'NONE',  ( -0.6592970117152722187, -7.499999799589161853, -434.1413533491637509 ) ) ;
#2893 = CARTESIAN_POINT ( 'NONE',  ( -39.23786858994942151, -8.000000000000000000, -387.8670522075712483 ) ) ;
#2894 = CARTESIAN_POINT ( 'NONE',  ( 2.381287040813000348E-07, -10.00000001404999850, 190.0000000000000000 ) ) ;
#2895 = CARTESIAN_POINT ( 'NONE',  ( -16.99996037728000076, 1.352916227065999958E-09, 314.9999801883000146 ) ) ;
#2896 = EDGE_CURVE ( 'NONE', #7412, #7389, #4983, .T. ) ;
#2897 = CARTESIAN_POINT ( 'NONE',  ( -7.006889269069000115, -6.844138725329000472, -284.9999999999999432 ) ) ;
#2898 = CARTESIAN_POINT ( 'NONE',  ( -16.34919249956382714, -2.583378889817198765, -315.0000000000000568 ) ) ;
#2899 = DIRECTION ( 'NONE',  ( 0.000000000000000000, 0.000000000000000000, 1.000000000000000000 ) ) ;
#2900 =( BOUNDED_SURFACE ( )  B_SPLINE_SURFACE ( 3, 1, ( 
 ( #6169, #2150 ),
 ( #3753, #3706 ),
 ( #9455, #5414 ),
 ( #6991, #2796 ) ),
 .UNSPECIFIED., .F., .F., .T. ) 
 B_SPLINE_SURFACE_WITH_KNOTS ( ( 4, 4 ),
 ( 2, 2 ),
 ( 0.000000000000000000, 1.000000000000000000 ),
 ( 0.000000000000000000, 1.000000000000000000 ),
 .UNSPECIFIED. ) 
 GEOMETRIC_REPRESENTATION_ITEM ( )  RATIONAL_B_SPLINE_SURFACE ( (
 ( 1.000000000000000000, 1.000000000000000000),
 ( 0.3333333333312610280, 0.3333333333312610280),
 ( 0.3333333333312610280, 0.3333333333312610280),
 ( 1.000000000000000000, 1.000000000000000000) ) ) 
 REPRESENTATION_ITEM ( '' )  SURFACE ( )  );
#2901 = DIRECTION ( 'NONE',  ( 0.000000000000000000, 1.000000000000000000, 0.000000000000000000 ) ) ;
#2902 = CARTESIAN_POINT ( 'NONE',  ( -2.301302514452984394, -7.114149834682999440, -436.1192177104634879 ) ) ;
#2903 = CARTESIAN_POINT ( 'NONE',  ( -11.28358823633008079, 7.096269052248557863, -315.0000000000001137 ) ) ;
#2904 = CARTESIAN_POINT ( 'NONE',  ( 18.14082875322000277, 3.150077164920001671, 190.0071920248299477 ) ) ;
#2905 = DIRECTION ( 'NONE',  ( 0.000000000000000000, -1.000000000000000000, 0.000000000000000000 ) ) ;
#2906 = ORIENTED_EDGE ( 'NONE', *, *, #6007, .F. ) ;
#2907 = CARTESIAN_POINT ( 'NONE',  ( 5.180828043054999554, -11.07085478567999992, -317.5000000000000000 ) ) ;
#2908 = AXIS2_PLACEMENT_3D ( 'NONE', #8831, #8134, #5760 ) ;
#2909 = EDGE_CURVE ( 'NONE', #2810, #1259, #8675, .T. ) ;
#2910 = DIRECTION ( 'NONE',  ( 0.1071946444232954182, 0.000000000000000000, -0.9942380540931651245 ) ) ;
#2911 = SURFACE_STYLE_USAGE ( .BOTH. , #5936 ) ;
#2912 = CARTESIAN_POINT ( 'NONE',  ( 16.31058353111865955, -2.657800654349994129, 315.0000000000000000 ) ) ;
#2913 = CARTESIAN_POINT ( 'NONE',  ( -4.031301020048999817, 9.630010295875997883, -314.6383426456000052 ) ) ;
#2914 = CYLINDRICAL_SURFACE ( 'NONE', #8484, 3.500000000000003997 ) ;
#2915 = CYLINDRICAL_SURFACE ( 'NONE', #8475, 5.000000000000004441 ) ;
#2916 = CARTESIAN_POINT ( 'NONE',  ( -24.51838671671999847, 2.500000000000000000, -497.7560445212000104 ) ) ;
#2917 = ORIENTED_EDGE ( 'NONE', *, *, #6163, .T. ) ;
#2918 = CARTESIAN_POINT ( 'NONE',  ( 18.77313104639999253, 1.494918992088000831, -317.4928077629770087 ) ) ;
#2919 = CIRCLE ( 'NONE', #6692, 3.500000000000003109 ) ;
#2920 = CARTESIAN_POINT ( 'NONE',  ( -14.97796429264999141, -8.396158284077998246, -317.0792622552969533 ) ) ;
#2921 = EDGE_CURVE ( 'NONE', #320, #8575, #6870, .T. ) ;
#2922 = CARTESIAN_POINT ( 'NONE',  ( 17.50000000000000000, -0.7437989020623000380, -315.0000000000000000 ) ) ;
#2923 = AXIS2_PLACEMENT_3D ( 'NONE', #2893, #9207, #8737 ) ;
#2924 = CARTESIAN_POINT ( 'NONE',  ( -3.644504295958682416, 9.783030308347003157, -314.5117835914683155 ) ) ;
#2925 = VERTEX_POINT ( 'NONE', #10248 ) ;
#2926 = CARTESIAN_POINT ( 'NONE',  ( -18.20814976352000158, -3.283820199526999772, 190.0000000000000000 ) ) ;
#2927 = CARTESIAN_POINT ( 'NONE',  ( -19.51225877040621981, -2.792229942217316019, 319.0000000000003979 ) ) ;
#2928 = ORIENTED_EDGE ( 'NONE', *, *, #10338, .F. ) ;
#2929 = CARTESIAN_POINT ( 'NONE',  ( 7.781240562249999826, -11.51887802030999985, 191.1197171614399792 ) ) ;
#2930 = ORIENTED_EDGE ( 'NONE', *, *, #407, .F. ) ;
#2931 = CARTESIAN_POINT ( 'NONE',  ( -16.04008061823806131, -3.141427272462999021, 315.0000000000000000 ) ) ;
#2932 = DIRECTION ( 'NONE',  ( 0.8820010751365675583, 0.000000000000000000, 0.4712473909295827323 ) ) ;
#2933 = EDGE_CURVE ( 'NONE', #4424, #5133, #6051, .T. ) ;
#2934 = CARTESIAN_POINT ( 'NONE',  ( 17.02428600387000301, 6.565037456673000982, 191.1197171614399792 ) ) ;
#2935 = DIRECTION ( 'NONE',  ( -0.7784864941890657919, 0.000000000000000000, -0.6276613564377031551 ) ) ;
#2936 = CARTESIAN_POINT ( 'NONE',  ( 19.57075148197997549, -0.3818783754278996523, -302.4229045757450081 ) ) ;
#2937 = CARTESIAN_POINT ( 'NONE',  ( 20.05691607070997051, 0.5615793767616999999, 319.5792614743400009 ) ) ;
#2938 = CARTESIAN_POINT ( 'NONE',  ( 14.28417481768999941, -5.042936695466000430, -315.0848619657999734 ) ) ;
#2939 = CARTESIAN_POINT ( 'NONE',  ( -17.36938240862999905, 0.02134527931160000100, 314.6383426456000052 ) ) ;
#2940 = ORIENTED_EDGE ( 'NONE', *, *, #9101, .T. ) ;
#2941 = CARTESIAN_POINT ( 'NONE',  ( -7.284698641071005731, -10.49877923466000063, 190.0071920248299477 ) ) ;
#2942 = CARTESIAN_POINT ( 'NONE',  ( -0.6337574957234999307, 12.50712592802002021, 318.8802828394900644 ) ) ;
#2943 = DIRECTION ( 'NONE',  ( 0.000000000000000000, -1.000000000000000000, 0.000000000000000000 ) ) ;
#2944 = CIRCLE ( 'NONE', #1233, 10.00000000000000000 ) ;
#2945 = PLANE ( 'NONE',  #10093 ) ;
#2946 = PLANE ( 'NONE',  #6232 ) ;
#2947 = CARTESIAN_POINT ( 'NONE',  ( -13.89435758465052828, 5.448822883216570823, 315.0000000000000568 ) ) ;
#2948 = CARTESIAN_POINT ( 'NONE',  ( -13.57573464316000056, -3.225916527208000151, 315.0000000000001705 ) ) ;
#2949 = CARTESIAN_POINT ( 'NONE',  ( -14.25125116527600078, -5.161338287358921306, -315.0000000000000568 ) ) ;
#2950 = CARTESIAN_POINT ( 'NONE',  ( -3.766936453924772277, -2.974863205562146007, -436.1437120911318743 ) ) ;
#2951 = CARTESIAN_POINT ( 'NONE',  ( -28.01838671672410896, -7.500000000000000000, -497.7560445212019999 ) ) ;
#2952 = CARTESIAN_POINT ( 'NONE',  ( -1.999999999997229772, -2.500000000000000000, -409.4999999999571969 ) ) ;
#2953 = CARTESIAN_POINT ( 'NONE',  ( -4.669917308725587191, 9.131001784561973977, -315.0000000000000000 ) ) ;
#2954 = PRODUCT_DEFINITION_SHAPE ( 'NONE', 'NONE',  #2522 ) ;
#2956 = CARTESIAN_POINT ( 'NONE',  ( 17.86997157320001151, 4.940892756443005851, 189.9229057364800042 ) ) ;
#2955 = AXIS2_PLACEMENT_3D ( 'NONE', #4423, #1246, #8449 ) ;
#2957 = LINE ( 'NONE', #6997, #6598 ) ;
#2958 = AXIS2_PLACEMENT_3D ( 'NONE', #7944, #9505, #7095 ) ;
#2959 = ORIENTED_EDGE ( 'NONE', *, *, #7600, .T. ) ;
#2960 = CARTESIAN_POINT ( 'NONE',  ( 17.62858316411999837, -4.302404616280000482, -317.5000000000030127 ) ) ;
#2961 = FACE_OUTER_BOUND ( 'NONE', #7228, .T. ) ;
#2962 = DIRECTION ( 'NONE',  ( 0.000000000000000000, 0.000000000000000000, 1.000000000000000000 ) ) ;
#2963 = CARTESIAN_POINT ( 'NONE',  ( 8.616673968646825443, -8.177724119443702477, 315.0000000000000000 ) ) ;
#2964 = CARTESIAN_POINT ( 'NONE',  ( -1.419551022038999966, 10.09154694854999867, -314.4150829855000211 ) ) ;
#2965 = DIRECTION ( 'NONE',  ( 0.000000000000000000, -1.000000000000000000, 0.000000000000000000 ) ) ;
#2966 = AXIS2_PLACEMENT_3D ( 'NONE', #5653, #774, #6466 ) ;
#2967 = CARTESIAN_POINT ( 'NONE',  ( 3.163121738623003054, 11.93735872977999968, 320.0770942683900557 ) ) ;
#2968 = CARTESIAN_POINT ( 'NONE',  ( -0.8331085234012651775, -2.500134501855002078, -434.2559579827629364 ) ) ;
#2969 = EDGE_LOOP ( 'NONE', ( #2366, #4306, #4136, #4911 ) ) ;
#2970 = CARTESIAN_POINT ( 'NONE',  ( -7.982667963825995194, 11.03627960042998701, -317.5770954168139610 ) ) ;
#2971 = CARTESIAN_POINT ( 'NONE',  ( 20.05670149355997722, 0.5623089763428997800, -317.0792622552969533 ) ) ;
#2972 = LINE ( 'NONE', #665, #5437 ) ;
#2973 = CARTESIAN_POINT ( 'NONE',  ( -2.000000000000000000, -10.50000000000000000, -409.5000000000000000 ) ) ;
#2974 = ORIENTED_EDGE ( 'NONE', *, *, #6930, .F. ) ;
#2975 = CARTESIAN_POINT ( 'NONE',  ( 19.49702808861182746, -2.833672667318399618, 319.0000000000003979 ) ) ;
#2976 = COLOUR_RGB ( '', 0.09019608, 0.27058824, 0.51372549) ;
#2977 = ORIENTED_EDGE ( 'NONE', *, *, #3168, .F. ) ;
#2978 = CARTESIAN_POINT ( 'NONE',  ( 12.80773887004084877, 9.614708322195337331, -316.5000000000004547 ) ) ;
#2979 = ORIENTED_EDGE ( 'NONE', *, *, #10090, .T. ) ;
#2980 =( BOUNDED_CURVE ( )  B_SPLINE_CURVE ( 3, ( #2119, #5187, #5237, #6195, #2927, #6966, #8512, #5285, #1255, #4533, #8460, #9332, #1154, #8558, #7712, #9481, #1204, #7758, #3947, #4757, #9534, #8137, #8888, #7280, #3784, #8026, #5606, #7071, #2390, #8941, #3140, #672, #7227, #10493, #1526, #4810, #562, #10339, #4645, #1478, #8081, #3196, #3029, #2975, #7978, #4862, #1585, #619 ),
 .UNSPECIFIED., .F., .F. ) 
 B_SPLINE_CURVE_WITH_KNOTS ( ( 4, 1, 1, 1, 1, 1, 1, 1, 1, 1, 1, 1, 1, 1, 1, 1, 1, 1, 1, 1, 1, 1, 1, 1, 1, 1, 1, 1, 1, 1, 1, 1, 1, 1, 1, 1, 1, 1, 1, 1, 1, 1, 1, 1, 1, 4 ),
 ( 0.000000000000000000, 0.01696016684112855444, 0.03526043942249579982, 0.05280277254187595859, 0.06993090526874458368, 0.08694163804313619071, 0.1040119350351715183, 0.1210139405588608608, 0.1379792171159070213, 0.1553986424958138379, 0.1736039501722520528, 0.1924119339504002102, 0.2116998327295473159, 0.2316504953696774671, 0.2523434511079291065, 0.2735071578860145403, 0.2951461022590910477, 0.3179819391660329009, 0.3428270683969382726, 0.3704763703089106741, 0.4013842106079443250, 0.4356267894623512271, 0.4731822280981954343, 0.5126799690798767850, 0.5516183454030080258, 0.5879427231221451278, 0.6209690717414463323, 0.6502633940987105898, 0.6759717312850139770, 0.6991685419836422000, 0.7210175260783882045, 0.7426211155567139510, 0.7640811388048153185, 0.7847659435495429880, 0.8046277674085308140, 0.8239473966552022244, 0.8426767883169219431, 0.8606205966378885908, 0.8779797588928679453, 0.8951189492511466561, 0.9121717320952801300, 0.9291919606104406260, 0.9463734364297033963, 0.9639783248497096890, 0.9823161612921426089, 1.000000000000000000 ),
 .UNSPECIFIED. ) 
 CURVE ( )  GEOMETRIC_REPRESENTATION_ITEM ( )  RATIONAL_B_SPLINE_CURVE ( ( 1.171573005652648991, 1.171573005652649213, 1.171573005652648991, 1.171573005652648991, 1.171573005652648991, 1.171573005652648991, 1.171573005652648991, 1.171573005652648991, 1.171573005652648991, 1.171573005652648991, 1.171573005652648991, 1.171573005652648991, 1.171573005652648991, 1.171573005652648991, 1.171573005652648991, 1.171573005652648991, 1.171573005652648991, 1.171573005652648991, 1.171573005652648991, 1.171573005652648991, 1.171573005652648991, 1.171573005652648991, 1.171573005652648991, 1.171573005652648991, 1.171573005652648991, 1.171573005652648991, 1.171573005652648991, 1.171573005652648991, 1.171573005652648991, 1.171573005652648991, 1.171573005652648991, 1.171573005652648991, 1.171573005652648991, 1.171573005652648991, 1.171573005652648991, 1.171573005652648991, 1.171573005652648991, 1.171573005652648991, 1.171573005652648991, 1.171573005652648991, 1.171573005652648991, 1.171573005652648991, 1.171573005652648991, 1.171573005652648991, 1.171573005652648991, 1.171573005652648991, 1.171573005652648991, 1.171573005652648991 ) ) 
 REPRESENTATION_ITEM ( '' )  );
#2981 = DIRECTION ( 'NONE',  ( -0.1071946444232958900, 0.000000000000000000, 0.9942380540931649024 ) ) ;
#2982 = CARTESIAN_POINT ( 'NONE',  ( 7.818484572095996121, -11.08186606788998674, -302.4229045757450081 ) ) ;
#2983 = DIRECTION ( 'NONE',  ( -0.1124491875265152124, 0.000000000000000000, 0.9936574763089273121 ) ) ;
#2984 = ORIENTED_EDGE ( 'NONE', *, *, #3202, .T. ) ;
#2985 = VECTOR ( 'NONE', #2901, 1000.000000000000000 ) ;
#2986 = CARTESIAN_POINT ( 'NONE',  ( -0.6600535743662629962, -7.458390606629000885, -434.6313374073768614 ) ) ;
#2987 = EDGE_CURVE ( 'NONE', #8626, #7650, #1211, .T. ) ;
#2988 = CARTESIAN_POINT ( 'NONE',  ( -16.88803284296001905, 5.077274453104001495, -302.5071922382879279 ) ) ;
#2989 = CARTESIAN_POINT ( 'NONE',  ( 14.74960734804001916, -8.445183187697006488, 318.8802828394900644 ) ) ;
#2990 = CARTESIAN_POINT ( 'NONE',  ( -8.519003879469000395, -8.390442916014999142, -314.8616023057000461 ) ) ;
#2991 = CARTESIAN_POINT ( 'NONE',  ( -1.388768300183999882, 9.421618921053999784, 315.0848619657999734 ) ) ;
#2992 = EDGE_CURVE ( 'NONE', #5421, #1962, #823, .T. ) ;
#2993 = ORIENTED_EDGE ( 'NONE', *, *, #7129, .F. ) ;
#2994 = CARTESIAN_POINT ( 'NONE',  ( -19.79199150660973672, -1.880421430186972165, 190.9999999999995737 ) ) ;
#2995 = CARTESIAN_POINT ( 'NONE',  ( -1.333798302234134647, -7.456821208003824530, -434.5634752832991694 ) ) ;
#2996 = DIRECTION ( 'NONE',  ( 0.000000000000000000, -1.000000000000000000, 0.000000000000000000 ) ) ;
#2997 = AXIS2_PLACEMENT_3D ( 'NONE', #7933, #9712, #1544 ) ;
#2998 = EDGE_CURVE ( 'NONE', #4191, #5439, #5397, .T. ) ;
#2999 = CARTESIAN_POINT ( 'NONE',  ( -1.999999999997229772, -7.500000000000000000, -409.4999999999571969 ) ) ;
#3000 =( LENGTH_UNIT ( ) NAMED_UNIT ( * ) SI_UNIT ( .MILLI., .METRE. ) );
#3001 = EDGE_CURVE ( 'NONE', #1085, #6747, #6203, .T. ) ;
#3002 = CARTESIAN_POINT ( 'NONE',  ( -91.84750071659622961, -2.366295999999999733, -370.2190357451694922 ) ) ;
#3003 = CARTESIAN_POINT ( 'NONE',  ( -20.00000000000000000, 3.518725546161979705E-10, 191.0000000000000000 ) ) ;
#3004 = CARTESIAN_POINT ( 'NONE',  ( -16.99996037728000076, 1.352916535802999941E-09, -314.9999801883000146 ) ) ;
#3005 = CARTESIAN_POINT ( 'NONE',  ( -11.69802267049820976, -4.081445891925754133, -438.6483114700716897 ) ) ;
#3006 = FILL_AREA_STYLE ('',( #9361 ) ) ;
#3007 = CARTESIAN_POINT ( 'NONE',  ( -12.67039042656561243, -5.789333632204900937, -439.0231271474323762 ) ) ;
#3008 = CARTESIAN_POINT ( 'NONE',  ( -2.450863364448387482, 9.399909383054032119, -315.0000000000000000 ) ) ;
#3009 = CARTESIAN_POINT ( 'NONE',  ( -11.98038374875001111, 9.553300872651998787, 189.9229057364800042 ) ) ;
#3010 = CARTESIAN_POINT ( 'NONE',  ( 1.604641703582619039, 9.999988110349836035, 314.4999449211996989 ) ) ;
#3011 = CARTESIAN_POINT ( 'NONE',  ( 6.353028986609323248, -4.484463380032637225, -524.9540790665465693 ) ) ;
#3012 = DIRECTION ( 'NONE',  ( -1.000000000000000000, 0.000000000000000000, 0.000000000000000000 ) ) ;
#3013 = ADVANCED_FACE ( 'NONE', ( #3690 ), #5514, .F. ) ;
#3014 = APPLICATION_PROTOCOL_DEFINITION ( 'draft international standard', 'automotive_design', 1998, #10183 ) ;
#3015 = CARTESIAN_POINT ( 'NONE',  ( 16.33370887135086491, -2.613387004688928261, 315.0000000000000568 ) ) ;
#3016 = CARTESIAN_POINT ( 'NONE',  ( 10.41198510038999991, 7.677033091942000453, -314.8616023057000461 ) ) ;
#3017 = CARTESIAN_POINT ( 'NONE',  ( -79.04021210711869116, -2.500000000000000000, -328.4066924704651456 ) ) ;
#3018 = CARTESIAN_POINT ( 'NONE',  ( 15.40147079910000372, 7.455286574312999903, 320.0770942683900557 ) ) ;
#3019 = SURFACE_STYLE_FILL_AREA ( #549 ) ;
#3020 = CARTESIAN_POINT ( 'NONE',  ( -0.8897543176725906111, -2.502046059794002186, -434.2898615358246843 ) ) ;
#3021 = ORIENTED_EDGE ( 'NONE', *, *, #6600, .T. ) ;
#3022 = CARTESIAN_POINT ( 'NONE',  ( -16.01024372474999069, 7.613620273433004293, -317.0792622552969533 ) ) ;
#3023 = PRODUCT_DEFINITION_FORMATION_WITH_SPECIFIED_SOURCE ( 'ANY', '', #4677, .NOT_KNOWN. ) ;
#3024 = FACE_OUTER_BOUND ( 'NONE', #5286, .T. ) ;
#3025 = DIRECTION ( 'NONE',  ( 1.000000000000000000, 0.000000000000000000, 0.000000000000000000 ) ) ;
#3026 = CARTESIAN_POINT ( 'NONE',  ( -37.62994892359998289, -8.000000000000000000, -402.7806230189686971 ) ) ;
#3027 = ORIENTED_EDGE ( 'NONE', *, *, #4829, .F. ) ;
#3028 = AXIS2_PLACEMENT_3D ( 'NONE', #2856, #8539, #5971 ) ;
#3029 = CARTESIAN_POINT ( 'NONE',  ( 19.12867493021229137, -3.682770601350499717, 319.0000000000003979 ) ) ;
#3030 = ORIENTED_EDGE ( 'NONE', *, *, #4040, .T. ) ;
#3031 = CARTESIAN_POINT ( 'NONE',  ( 4.978134047761749947, 12.12024670600909282, -316.5000000000004547 ) ) ;
#3032 = ORIENTED_EDGE ( 'NONE', *, *, #7790, .F. ) ;
#3033 = CARTESIAN_POINT ( 'NONE',  ( -2.450606348566487735, -9.399923241459493539, 315.0000000000000568 ) ) ;
#3034 = CARTESIAN_POINT ( 'NONE',  ( -13.92883798546999508, -9.075834183867002025, -302.9207377450070453 ) ) ;
#3035 = LINE ( 'NONE', #1424, #7979 ) ;
#3036 = EDGE_CURVE ( 'NONE', #3804, #6040, #6024, .T. ) ;
#3037 = CARTESIAN_POINT ( 'NONE',  ( -15.69672544750998888, 7.226176219113002119, -302.4229045757450081 ) ) ;
#3038 =( REPRESENTATION_RELATIONSHIP ('NONE','NONE', #8468, #1832 ) REPRESENTATION_RELATIONSHIP_WITH_TRANSFORMATION ( #221 )SHAPE_REPRESENTATION_RELATIONSHIP( ) );
#3039 = DIRECTION ( 'NONE',  ( 0.000000000000000000, -1.000000000000000000, 0.000000000000000000 ) ) ;
#3040 = ORIENTED_EDGE ( 'NONE', *, *, #9427, .F. ) ;
#3041 = CARTESIAN_POINT ( 'NONE',  ( -14.67553856548000013, -5.592168771406000438, -314.4150829855000211 ) ) ;
#3042 = CARTESIAN_POINT ( 'NONE',  ( -19.99999036626000048, -4.642009783819999925E-09, -316.5000000000000000 ) ) ;
#3043 = EDGE_LOOP ( 'NONE', ( #7539, #5201 ) ) ;
#3044 = CARTESIAN_POINT ( 'NONE',  ( -8.712128322569002492, -10.82186910204999997, 189.9229057364800042 ) ) ;
#3045 = TOROIDAL_SURFACE ( 'NONE', #5961, 20.50000000000000000, 0.5000000000000000000 ) ;
#3046 = CARTESIAN_POINT ( 'NONE',  ( -16.34529002343606052, 7.216405960070773951, 190.9999999999996589 ) ) ;
#3047 = DIRECTION ( 'NONE',  ( 0.000000000000000000, 0.000000000000000000, -1.000000000000000000 ) ) ;
#3048 = ADVANCED_FACE ( 'NONE', ( #1081 ), #6843, .T. ) ;
#3049 = EDGE_CURVE ( 'NONE', #4096, #4227, #1159, .T. ) ;
#3050 = CARTESIAN_POINT ( 'NONE',  ( -14.67553856548000013, -5.592168771406000438, 314.4150829855000211 ) ) ;
#3051 = LINE ( 'NONE', #6219, #4361 ) ;
#3052 = VECTOR ( 'NONE', #8481, 1000.000000000000000 ) ;
#3053 = CARTESIAN_POINT ( 'NONE',  ( -46.74071243419621169, -8.000000000000000000, -414.3237589990241077 ) ) ;
#3054 = CARTESIAN_POINT ( 'NONE',  ( -7.560581757588001217, -10.42594579828999990, 319.9928079742500131 ) ) ;
#3055 = CARTESIAN_POINT ( 'NONE',  ( -5.334282155825492033, -9.025044196641820449, -314.9999999999999432 ) ) ;
#3056 = SURFACE_SIDE_STYLE ('',( #10414 ) ) ;
#3057 = CARTESIAN_POINT ( 'NONE',  ( 11.28781796570999951, 4.951468039558000633, 315.0000000000000000 ) ) ;
#3058 = ORIENTED_EDGE ( 'NONE', *, *, #7135, .T. ) ;
#3059 = DIRECTION ( 'NONE',  ( 0.000000000000000000, 1.000000000000000000, -0.000000000000000000 ) ) ;
#3060 = CARTESIAN_POINT ( 'NONE',  ( 4.461988713456979561, 9.163769885065249809, -314.9999999999999432 ) ) ;
#3061 = CARTESIAN_POINT ( 'NONE',  ( -18.75323799499002675, 4.519634888734000100, 190.4207385301700128 ) ) ;
#3062 = CARTESIAN_POINT ( 'NONE',  ( -10.23467949614885697, 10.00000000050611781, -302.5000000000003979 ) ) ;
#3063 = EDGE_CURVE ( 'NONE', #9535, #4497, #8204, .T. ) ;
#3064 = CARTESIAN_POINT ( 'NONE',  ( 11.71572875766478639, -12.49999999885353041, -316.5000000000000000 ) ) ;
#3065 = DIRECTION ( 'NONE',  ( -0.2381566831044910626, 0.000000000000000000, 0.9712267471052612455 ) ) ;
#3066 = DIRECTION ( 'NONE',  ( 0.8371691043312221581, -7.069190062780585386E-17, 0.5469441386039887165 ) ) ;
#3067 = CARTESIAN_POINT ( 'NONE',  ( -9.314945463565893036, -11.07333627012143396, -303.4999999999996589 ) ) ;
#3068 = CARTESIAN_POINT ( 'NONE',  ( 17.12450099635000100, -0.4005340032738999856, -314.8616023057000461 ) ) ;
#3069 = CARTESIAN_POINT ( 'NONE',  ( 17.40348243411531826, -5.898854857574459487, 314.4999507458385892 ) ) ;
#3070 = CARTESIAN_POINT ( 'NONE',  ( -19.59086175841999378, 0.09594170647769999227, 320.0770942683900557 ) ) ;
#3071 = CARTESIAN_POINT ( 'NONE',  ( -14.83733877544362478, -5.575412435490171070, -439.0269195386780439 ) ) ;
#3072 = CARTESIAN_POINT ( 'NONE',  ( -1.729952635784063331, -2.694803404275001313, -435.0907047969546966 ) ) ;
#3073 = ORIENTED_EDGE ( 'NONE', *, *, #597, .F. ) ;
#3074 = CARTESIAN_POINT ( 'NONE',  ( -6.660995095996002924, 11.36691212455000333, -317.5770954168139610 ) ) ;
#3075 = DIRECTION ( 'NONE',  ( -0.2381566831044917565, 0.000000000000000000, 0.9712267471052610235 ) ) ;
#3076 = AXIS2_PLACEMENT_3D ( 'NONE', #8078, #773, #7383 ) ;
#3077 = VERTEX_POINT ( 'NONE', #8542 ) ;
#3078 = DIRECTION ( 'NONE',  ( -0.9921831154218023752, 0.000000000000000000, -0.1247904863035890627 ) ) ;
#3079 = CARTESIAN_POINT ( 'NONE',  ( -12.32405526929588291, 7.045528031251309997, -314.5741454722275421 ) ) ;
#3080 = ORIENTED_EDGE ( 'NONE', *, *, #3319, .F. ) ;
#3081 = CIRCLE ( 'NONE', #7887, 0.5000000000000004441 ) ;
#3082 = CARTESIAN_POINT ( 'NONE',  ( -13.47608353327723485, -6.291341891605536141, -314.5797986957608146 ) ) ;
#3083 = ORIENTED_EDGE ( 'NONE', *, *, #9291, .F. ) ;
#3084 = CARTESIAN_POINT ( 'NONE',  ( -2.055855549839187280, 12.45069410617974448, -316.5000000000004547 ) ) ;
#3085 = ORIENTED_EDGE ( 'NONE', *, *, #5584, .T. ) ;
#3086 = CARTESIAN_POINT ( 'NONE',  ( -7.042505780985288233, -8.656073623659681360, 315.0000000000000000 ) ) ;
#3087 = CARTESIAN_POINT ( 'NONE',  ( -10.38823308980000704, -10.24279834975000192, -302.4229045757450081 ) ) ;
#3088 = LINE ( 'NONE', #1533, #9854 ) ;
#3089 = VERTEX_POINT ( 'NONE', #2704 ) ;
#3090 = STYLED_ITEM ( 'NONE', ( #5640 ), #8714 ) ;
#3091 =( NAMED_UNIT ( * ) PLANE_ANGLE_UNIT ( ) SI_UNIT ( $, .RADIAN. ) );
#3092 = CARTESIAN_POINT ( 'NONE',  ( 0.1616652313949000219, 12.09676013415999485, -302.4229045757450081 ) ) ;
#3093 = CARTESIAN_POINT ( 'NONE',  ( -14.04143820182998503, -8.903536631273988533, 318.8802828394900644 ) ) ;
#3094 = VERTEX_POINT ( 'NONE', #2599 ) ;
#3095 = CARTESIAN_POINT ( 'NONE',  ( -3.932702496464000497, -9.868769537474999964, -314.4150829855000211 ) ) ;
#3096 = CARTESIAN_POINT ( 'NONE',  ( 10.18931492271999950, 9.698324433322001781, -302.5000000000000000 ) ) ;
#3097 = EDGE_LOOP ( 'NONE', ( #1420, #7294, #6137, #4139 ) ) ;
#3098 = CARTESIAN_POINT ( 'NONE',  ( -12.81613682183999536, -9.130924732858002102, 189.9229057364800042 ) ) ;
#3099 = CARTESIAN_POINT ( 'NONE',  ( -19.99999721801999897, -7.771324026006999692E-11, 191.0000000000000000 ) ) ;
#3100 = DIRECTION ( 'NONE',  ( 0.000000000000000000, 1.000000000000000000, 0.000000000000000000 ) ) ;
#3101 = ADVANCED_FACE ( 'NONE', ( #8341 ), #4266, .T. ) ;
#3102 = EDGE_LOOP ( 'NONE', ( #6612, #162 ) ) ;
#3103 = CARTESIAN_POINT ( 'NONE',  ( -8.450675645183000739, -8.177559542660000957, 315.0848619657999734 ) ) ;
#3104 = FILL_AREA_STYLE_COLOUR ( '', #10193 ) ;
#3105 = CARTESIAN_POINT ( 'NONE',  ( 16.29068328802999943, 5.892689959824000567, 320.0000000000000000 ) ) ;
#3106 = CARTESIAN_POINT ( 'NONE',  ( -17.30539973653000629, -4.527429531397997309, 319.9928079742500131 ) ) ;
#3107 = CARTESIAN_POINT ( 'NONE',  ( 19.38368284813939013, -7.500000000000000000, -515.5999187775453265 ) ) ;
#3108 = ADVANCED_FACE ( 'NONE', ( #10065 ), #6896, .T. ) ;
#3109 = FACE_OUTER_BOUND ( 'NONE', #6004, .T. ) ;
#3110 = ORIENTED_EDGE ( 'NONE', *, *, #7485, .T. ) ;
#3111 = CARTESIAN_POINT ( 'NONE',  ( 28.53863984632670636, -2.500000000000000000, -506.8274460463252353 ) ) ;
#3112 = VECTOR ( 'NONE', #3078, 1000.000000000000114 ) ;
#3113 = ADVANCED_FACE ( 'NONE', ( #1897 ), #5367, .T. ) ;
#3114 = CARTESIAN_POINT ( 'NONE',  ( 19.56991616969001058, -0.3941640562313002416, 189.9229057364800042 ) ) ;
#3115 = CARTESIAN_POINT ( 'NONE',  ( 9.995120280747379127, 8.217201865419340834, 314.4999464406708967 ) ) ;
#3116 = CARTESIAN_POINT ( 'NONE',  ( 20.00000000000000000, 4.642020101641720348E-09, -316.5000000000000000 ) ) ;
#3117 = CARTESIAN_POINT ( 'NONE',  ( 17.50000000000000711, -8.653813013134384923E-10, -302.5000000000000568 ) ) ;
#3118 = SHAPE_DEFINITION_REPRESENTATION ( #9474, #7381 ) ;
#3119 = CARTESIAN_POINT ( 'NONE',  ( -13.88908508137762077, -9.009716997455477383, -303.4999999999996589 ) ) ;
#3120 = CARTESIAN_POINT ( 'NONE',  ( -18.99987386368999864, -0.5560526133780999691, -302.5000000001010108 ) ) ;
#3121 = ADVANCED_FACE ( 'NONE', ( #4682 ), #10373, .T. ) ;
#3122 = CARTESIAN_POINT ( 'NONE',  ( -72.90663470102438737, -7.500000000000000888, -371.7168990826883714 ) ) ;
#3123 = AXIS2_PLACEMENT_3D ( 'NONE', #2284, #3198, #8776 ) ;
#3124 = CARTESIAN_POINT ( 'NONE',  ( -9.773738012405997821, 10.46865777734000424, 320.0770942683900557 ) ) ;
#3125 = EDGE_CURVE ( 'NONE', #6593, #7069, #10600, .T. ) ;
#3126 = CARTESIAN_POINT ( 'NONE',  ( -0.7288599747256179207, -2.498024261830999571, -434.1773087478343314 ) ) ;
#3127 = ORIENTED_EDGE ( 'NONE', *, *, #6034, .T. ) ;
#3128 = CARTESIAN_POINT ( 'NONE',  ( 9.065820074235004356, 10.71255845790999572, -317.5770954168139610 ) ) ;
#3129 = CARTESIAN_POINT ( 'NONE',  ( -20.01656911870001920, -0.3693805509907998053, -316.3802825947000201 ) ) ;
#3130 = PRODUCT_DEFINITION_SHAPE ( 'NONE', 'NONE',  #3963 ) ;
#3131 = EDGE_LOOP ( 'NONE', ( #791, #3679 ) ) ;
#3132 = DIRECTION ( 'NONE',  ( 1.000000000000000000, 0.000000000000000000, 0.000000000000000000 ) ) ;
#3133 = EDGE_CURVE ( 'NONE', #10390, #9641, #5424, .T. ) ;
#3134 = VECTOR ( 'NONE', #264, 1000.000000000000000 ) ;
#3135 = PRODUCT_DEFINITION_CONTEXT ( 'detailed design', #2153, 'design' ) ;
#3136 = B_SPLINE_CURVE_WITH_KNOTS ( 'NONE', 3,
 ( #1244, #2109, #2863, #4520 ),
 .UNSPECIFIED., .F., .F.,
 ( 4, 4 ),
 ( 0.000000000000000000, 1.000000000000000000 ),
 .UNSPECIFIED. ) ;
#3137 = DIRECTION ( 'NONE',  ( -0.1071946444232958900, 0.000000000000000000, 0.9942380540931649024 ) ) ;
#3138 = DIRECTION ( 'NONE',  ( -0.9612616959383299964, 0.000000000000000000, -0.2756373558169601945 ) ) ;
#3139 = ORIENTED_EDGE ( 'NONE', *, *, #309, .T. ) ;
#3140 = CARTESIAN_POINT ( 'NONE',  ( 9.914941699848354162, -10.86515064494810545, 319.0000000000003979 ) ) ;
#3141 = VERTEX_POINT ( 'NONE', #1294 ) ;
#3142 = FACE_OUTER_BOUND ( 'NONE', #9330, .T. ) ;
#3143 = ORIENTED_EDGE ( 'NONE', *, *, #10338, .T. ) ;
#3144 = CARTESIAN_POINT ( 'NONE',  ( -14.08994485310920730, -5.290256584484003710, 314.9999999999999432 ) ) ;
#3145 = CARTESIAN_POINT ( 'NONE',  ( -0.1616652313949000219, -12.09676013415999485, -302.4229045757450081 ) ) ;
#3146 = CARTESIAN_POINT ( 'NONE',  ( -33.34106825788445150, -2.500000000000000000, -439.6766126514281154 ) ) ;
#3147 = LINE ( 'NONE', #733, #9358 ) ;
#3148 = CARTESIAN_POINT ( 'NONE',  ( -10.54839116401999988, 10.71567991178000057, -302.9207377450070453 ) ) ;
#3149 = EDGE_CURVE ( 'NONE', #574, #722, #1045, .T. ) ;
#3150 = CIRCLE ( 'NONE', #9164, 14.99999999999999112 ) ;
#3151 = CARTESIAN_POINT ( 'NONE',  ( 18.68148959551998445, -4.475099553145003739, 318.8802828394900644 ) ) ;
#3152 = ORIENTED_EDGE ( 'NONE', *, *, #682, .F. ) ;
#3153 = CARTESIAN_POINT ( 'NONE',  ( -11.89238025184999792, -6.701939844102000166, -315.0848619657999734 ) ) ;
#3154 = CARTESIAN_POINT ( 'NONE',  ( -7.895350322666780940, -9.000000000000001776, -398.4775300148504016 ) ) ;
#3155 = ORIENTED_EDGE ( 'NONE', *, *, #9756, .F. ) ;
#3156 = CARTESIAN_POINT ( 'NONE',  ( -19.59059457349998823, -0.06993619660353000977, 189.9229057364800042 ) ) ;
#3157 = CARTESIAN_POINT ( 'NONE',  ( -8.518317708839887814, -2.500000000000000000, -528.6824739677025491 ) ) ;
#3158 = CARTESIAN_POINT ( 'NONE',  ( -8.586595388443328147, -2.500000000000000000, -526.6836397678595176 ) ) ;
#3159 = COLOUR_RGB ( '', 0.66274510, 0.83137255, 0.94901961) ;
#3160 = CARTESIAN_POINT ( 'NONE',  ( -6.273744347102000241, -8.772995918477999311, 315.0848619657999734 ) ) ;
#3161 = DIRECTION ( 'NONE',  ( 1.000000000000000000, 0.000000000000000000, 0.000000000000000000 ) ) ;
#3162 = VECTOR ( 'NONE', #1973, 1000.000000000000000 ) ;
#3163 = CARTESIAN_POINT ( 'NONE',  ( -16.26474538691000049, 5.919460245093000061, 320.0000000000000000 ) ) ;
#3164 = CARTESIAN_POINT ( 'NONE',  ( -0.3140675329811673522, -8.000000000000000000, -361.6501536237392429 ) ) ;
#3165 = LINE ( 'NONE', #3107, #6217 ) ;
#3166 = CARTESIAN_POINT ( 'NONE',  ( -17.50000000088855501, -5.867334121986932161, -302.5000000000001705 ) ) ;
#3167 = DIRECTION ( 'NONE',  ( 0.6364744784326697991, 0.000000000000000000, -0.7712977624133632304 ) ) ;
#3168 = EDGE_CURVE ( 'NONE', #4480, #5049, #3226, .T. ) ;
#3169 = ORIENTED_EDGE ( 'NONE', *, *, #3440, .F. ) ;
#3170 = LINE ( 'NONE', #6444, #211 ) ;
#3171 = VECTOR ( 'NONE', #7340, 1000.000000000000000 ) ;
#3172 = CARTESIAN_POINT ( 'NONE',  ( 9.832070176257998284, 10.44777315889000313, 189.9229057364800042 ) ) ;
#3173 = DIRECTION ( 'NONE',  ( 0.8820010751365675583, 0.000000000000000000, 0.4712473909295827323 ) ) ;
#3174 = DIRECTION ( 'NONE',  ( -1.000000000000000000, 0.000000000000000000, 0.000000000000000000 ) ) ;
#3175 = AXIS2_PLACEMENT_3D ( 'NONE', #2875, #513, #9384 ) ;
#3176 = COLOUR_RGB ( '', 0.40784314, 0.44705882, 0.49803922) ;
#3177 = CARTESIAN_POINT ( 'NONE',  ( -19.99998650234397957, 8.894530543673175064E-07, -302.9142199863263158 ) ) ;
#3178 = CARTESIAN_POINT ( 'NONE',  ( 12.85811403544582099, -9.588400772462145838, -303.5000000000006253 ) ) ;
#3179 = CARTESIAN_POINT ( 'NONE',  ( 16.89608781496000134, 0.5923740909019999945, -315.0848619657999734 ) ) ;
#3180 = PLANE ( 'NONE',  #9106 ) ;
#3181 = CARTESIAN_POINT ( 'NONE',  ( -18.99998114578000141, 0.3144692935366000253, 190.0000000000100044 ) ) ;
#3182 = CARTESIAN_POINT ( 'NONE',  ( 19.56990143371999125, -0.3944980022354002136, 320.0770942683900557 ) ) ;
#3183 = DIRECTION ( 'NONE',  ( 0.7426245373610016465, 0.000000000000000000, -0.6697079934638365817 ) ) ;
#3184 = CARTESIAN_POINT ( 'NONE',  ( -0.7166823250270980550, -2.498181146152001819, -434.1608823843793061 ) ) ;
#3185 = ORIENTED_EDGE ( 'NONE', *, *, #4369, .T. ) ;
#3186 = CARTESIAN_POINT ( 'NONE',  ( 15.92039057294001125, 7.578271297757998681, -316.3802825947000201 ) ) ;
#3187 = CARTESIAN_POINT ( 'NONE',  ( -12.80442074722001067, -9.608322671940996429, -316.3802825947000201 ) ) ;
#3188 = STYLED_ITEM ( 'NONE', ( #7767 ), #5834 ) ;
#3189 = ADVANCED_FACE ( 'NONE', ( #2858 ), #4464, .T. ) ;
#3190 = CARTESIAN_POINT ( 'NONE',  ( 13.36276382026999876, -8.154196903800000840, 320.0000000000000000 ) ) ;
#3191 = CARTESIAN_POINT ( 'NONE',  ( -0.2949131312215419465, -7.545445293999001990, -434.0704074631209437 ) ) ;
#3192 = PLANE ( 'NONE',  #5139 ) ;
#3193 = CARTESIAN_POINT ( 'NONE',  ( -85.79375217459825365, -7.500000000000000000, -343.3529193039154279 ) ) ;
#3194 = VERTEX_POINT ( 'NONE', #8590 ) ;
#3195 = CARTESIAN_POINT ( 'NONE',  ( -0.5535498271043974849, -7.499999952522999891, -434.2938920418101816 ) ) ;
#3196 = CARTESIAN_POINT ( 'NONE',  ( 18.68762439754708637, -4.478870766961967398, 319.0000000000003979 ) ) ;
#3197 = ORIENTED_EDGE ( 'NONE', *, *, #1024, .F. ) ;
#3198 = DIRECTION ( 'NONE',  ( 0.000000000000000000, 1.000000000000000000, -0.000000000000000000 ) ) ;
#3199 = ORIENTED_EDGE ( 'NONE', *, *, #6021, .F. ) ;
#3200 = CARTESIAN_POINT ( 'NONE',  ( -1.573733331195987573, -9.469132543440894167, 315.0000000000001137 ) ) ;
#3201 = CARTESIAN_POINT ( 'NONE',  ( -19.56012101500002132, 0.5268190066377996805, -302.4229045757450081 ) ) ;
#3202 = EDGE_CURVE ( 'NONE', #7283, #289, #494, .T. ) ;
#3203 = DIRECTION ( 'NONE',  ( -0.000000000000000000, 1.000000000000000000, 0.000000000000000000 ) ) ;
#3204 = ADVANCED_FACE ( 'NONE', ( #544 ), #2158, .F. ) ;
#3205 = FACE_OUTER_BOUND ( 'NONE', #7577, .T. ) ;
#3206 = SURFACE_STYLE_FILL_AREA ( #883 ) ;
#3207 = CARTESIAN_POINT ( 'NONE',  ( 19.37583693248997108, 3.422417436021003123, -302.9207377450070453 ) ) ;
#3208 = CYLINDRICAL_SURFACE ( 'NONE', #5655, 0.5000000000000083267 ) ;
#3209 = EDGE_LOOP ( 'NONE', ( #3058, #3445, #4855, #6669, #927, #4767, #7906 ) ) ;
#3210 = CARTESIAN_POINT ( 'NONE',  ( 8.620760283086999820, -8.357092890497000326, -314.8616023057000461 ) ) ;
#3211 = DIRECTION ( 'NONE',  ( -5.235554895604999868E-10, -4.130579097307000442E-10, 1.000000000000000000 ) ) ;
#3212 = EDGE_LOOP ( 'NONE', ( #5791, #6114, #6899, #4274 ) ) ;
#3213 = CARTESIAN_POINT ( 'NONE',  ( -18.86321946521001180, 0.4765678057151996327, 190.0071920248299477 ) ) ;
#3214 = CARTESIAN_POINT ( 'NONE',  ( 19.14871320452657599, 3.641870911972380220, 190.9999999999996589 ) ) ;
#3215 = DIRECTION ( 'NONE',  ( -1.000000000000000000, 0.000000000000000000, 0.000000000000000000 ) ) ;
#3216 = EDGE_CURVE ( 'NONE', #146, #2925, #1238, .T. ) ;
#3217 = CARTESIAN_POINT ( 'NONE',  ( -17.20518503178000103, -1.389427005613000032, 314.6383426456000052 ) ) ;
#3218 = CARTESIAN_POINT ( 'NONE',  ( -2.579601697407999605, 11.41110358643000033, 320.0000000000000000 ) ) ;
#3219 = DIRECTION ( 'NONE',  ( 0.1071946444232959872, 0.000000000000000000, -0.9942380540931649024 ) ) ;
#3220 = AXIS2_PLACEMENT_3D ( 'NONE', #9198, #7573, #219 ) ;
#3221 = CARTESIAN_POINT ( 'NONE',  ( -6.040317665795909008, 11.93081507280031239, 319.0000000000005116 ) ) ;
#3222 = CARTESIAN_POINT ( 'NONE',  ( -14.81438263496213814, -4.470068862813207922, -439.1205369730296297 ) ) ;
#3223 = DIRECTION ( 'NONE',  ( -0.000000000000000000, 1.000000000000000000, 0.000000000000000000 ) ) ;
#3224 = VERTEX_POINT ( 'NONE', #7055 ) ;
#3225 = DIRECTION ( 'NONE',  ( 0.000000000000000000, -1.000000000000000000, 0.000000000000000000 ) ) ;
#3226 = CIRCLE ( 'NONE', #9243, 11.00000000000000000 ) ;
#3227 = CARTESIAN_POINT ( 'NONE',  ( -20.00000000068207129, -7.322330470855613171, -316.5000000000000000 ) ) ;
#3228 = FACE_OUTER_BOUND ( 'NONE', #3258, .T. ) ;
#3229 = APPLICATION_PROTOCOL_DEFINITION ( 'draft international standard', 'automotive_design', 1998, #9006 ) ;
#3230 = CARTESIAN_POINT ( 'NONE',  ( 11.72170966038013162, -10.14138702413947790, -303.4999999999996589 ) ) ;
#3231 = CARTESIAN_POINT ( 'NONE',  ( -28.01838671672000203, -2.500000000000000000, -497.7560445212000104 ) ) ;
#3232 = FACE_OUTER_BOUND ( 'NONE', #2101, .T. ) ;
#3233 = CARTESIAN_POINT ( 'NONE',  ( -3.707567269721498526, -7.033586184390685503, -436.1197384410193081 ) ) ;
#3234 = CARTESIAN_POINT ( 'NONE',  ( 19.98292278601002181, -0.4165571180016003350, 318.8802828394900644 ) ) ;
#3235 = PRESENTATION_STYLE_ASSIGNMENT (( #3398 ) ) ;
#3236 = CARTESIAN_POINT ( 'NONE',  ( -0.9356534891085935834, -2.545231261524000033, -435.0024077940244638 ) ) ;
#3237 = CARTESIAN_POINT ( 'NONE',  ( -14.37110465573396212, -2.500000000000000000, -348.9812360766022721 ) ) ;
#3238 = CARTESIAN_POINT ( 'NONE',  ( 6.484736462136006629, 11.91614536315999828, -317.0792622552969533 ) ) ;
#3239 = CARTESIAN_POINT ( 'NONE',  ( -13.30825372127758399, -9.500000000000001776, -400.6612558711213410 ) ) ;
#3240 = ADVANCED_FACE ( 'NONE', ( #2961 ), #6950, .F. ) ;
#3241 = CARTESIAN_POINT ( 'NONE',  ( -4.804283134583999804, -11.13634285072000019, 320.0000000000000000 ) ) ;
#3242 = CARTESIAN_POINT ( 'NONE',  ( -1.837856579518353906, -7.344572662436001487, -434.9059567300546973 ) ) ;
#3243 = DIRECTION ( 'NONE',  ( 1.000000000000000000, 0.000000000000000000, 0.000000000000000000 ) ) ;
#3244 = CARTESIAN_POINT ( 'NONE',  ( -1.669371716897545710, -9.454742746653563401, -315.0000000000000000 ) ) ;
#3245 = ORIENTED_EDGE ( 'NONE', *, *, #2698, .T. ) ;
#3246 = CARTESIAN_POINT ( 'NONE',  ( -12.98706127646999953, 6.788989183774999603, -315.0000000000001137 ) ) ;
#3247 = EDGE_LOOP ( 'NONE', ( #4992, #9977, #8474, #1048 ) ) ;
#3248 = CARTESIAN_POINT ( 'NONE',  ( -16.14934711101999909, 6.043101335943000585, -317.5000000000000000 ) ) ;
#3249 = ORIENTED_EDGE ( 'NONE', *, *, #5471, .F. ) ;
#3250 = CARTESIAN_POINT ( 'NONE',  ( 1.678162365823997915, -12.55068027652000140, -302.9207377450070453 ) ) ;
#3251 = EDGE_CURVE ( 'NONE', #8202, #5927, #9519, .T. ) ;
#3252 = FACE_OUTER_BOUND ( 'NONE', #1655, .T. ) ;
#3253 = CARTESIAN_POINT ( 'NONE',  ( -19.63511402242541237, -8.000000000000000000, -416.9332195861426840 ) ) ;
#3254 = AXIS2_PLACEMENT_3D ( 'NONE', #4212, #4371, #1031 ) ;
#3255 = CIRCLE ( 'NONE', #171, 12.50000000000001421 ) ;
#3256 = CARTESIAN_POINT ( 'NONE',  ( 7.921361508960999664, 11.05315760980000661, -302.4229045757450081 ) ) ;
#3257 = LINE ( 'NONE', #4281, #5489 ) ;
#3258 = EDGE_LOOP ( 'NONE', ( #5813, #4124, #3127, #7270 ) ) ;
#3259 = CARTESIAN_POINT ( 'NONE',  ( -16.78232460783999969, -3.056336161456999712, -314.4150829855000211 ) ) ;
#3260 = ADVANCED_FACE ( 'NONE', ( #1398, #604 ), #3877, .T. ) ;
#3261 = CARTESIAN_POINT ( 'NONE',  ( -16.90171868104999930, -0.3834349726278000192, 315.0848619657999734 ) ) ;
#3262 = VERTEX_POINT ( 'NONE', #2051 ) ;
#3263 = CARTESIAN_POINT ( 'NONE',  ( -14.91611818836001824, -6.947523351336002406, 190.0071920248299477 ) ) ;
#3264 = CARTESIAN_POINT ( 'NONE',  ( 19.99996770037257221, 0.3054858693455833052, 190.9999999999996589 ) ) ;
#3265 = DIRECTION ( 'NONE',  ( -0.7784864941890659029, 0.000000000000000000, -0.6276613564377032661 ) ) ;
#3266 = CARTESIAN_POINT ( 'NONE',  ( -2.000000000003786749, -8.000000000000000000, -409.4999999999758415 ) ) ;
#3267 = AXIS2_PLACEMENT_3D ( 'NONE', #8898, #3039, #524 ) ;
#3268 = CARTESIAN_POINT ( 'NONE',  ( -16.39086977655999888, -2.839079766962000040, 314.8616023057000461 ) ) ;
#3269 = SHAPE_REPRESENTATION_RELATIONSHIP ( 'NONE' , 'NONE' ,  #7381, #8498 ) ;
#3270 = CARTESIAN_POINT ( 'NONE',  ( -5.939701018627000728, 10.93065061464000109, 320.0000000000000000 ) ) ;
#3271 = CARTESIAN_POINT ( 'NONE',  ( 9.773738012405997821, -10.46865777734000424, 320.0770942683900557 ) ) ;
#3272 = CARTESIAN_POINT ( 'NONE',  ( -4.393607043691841518, 12.21170385155075344, 319.0000000000005116 ) ) ;
#3273 = CARTESIAN_POINT ( 'NONE',  ( -0.3764627761248945381, -7.500000000000000888, -361.1540620660322816 ) ) ;
#3274 = LINE ( 'NONE', #2365, #5569 ) ;
#3275 = VECTOR ( 'NONE', #3747, 1000.000000000000000 ) ;
#3276 = ORIENTED_EDGE ( 'NONE', *, *, #7206, .F. ) ;
#3277 = CARTESIAN_POINT ( 'NONE',  ( -15.54870946350325767, -2.500000000000000000, -436.1258788022018393 ) ) ;
#3278 = DIRECTION ( 'NONE',  ( 0.000000000000000000, -1.000000000000000000, -0.000000000000000000 ) ) ;
#3279 = CARTESIAN_POINT ( 'NONE',  ( 13.12098914876195366, 6.031629431400056696, 314.9999999999999432 ) ) ;
#3280 = CARTESIAN_POINT ( 'NONE',  ( -17.50000000000000000, 0.000000000000000000, -315.0000000000000000 ) ) ;
#3281 = CARTESIAN_POINT ( 'NONE',  ( -18.32212638522000248, -3.124911926288000075, -302.5000000000129603 ) ) ;
#3282 = CARTESIAN_POINT ( 'NONE',  ( -5.399293614865643853, -7.500000000000000000, -410.3335483908228980 ) ) ;
#3283 = CARTESIAN_POINT ( 'NONE',  ( -8.369756866907680504, -6.378185918057877934, -437.7466453813695466 ) ) ;
#3284 = LINE ( 'NONE', #2324, #7395 ) ;
#3285 = CARTESIAN_POINT ( 'NONE',  ( -81.20226567874760804, -2.366295999999999733, -347.7024309728756748 ) ) ;
#3286 = VERTEX_POINT ( 'NONE', #5317 ) ;
#3287 = CARTESIAN_POINT ( 'NONE',  ( 15.97383562432999149, 7.643564190274003245, -317.0792622552969533 ) ) ;
#3288 = CARTESIAN_POINT ( 'NONE',  ( -0.3764627761248945381, -12.00000000000000000, -361.1540620660322816 ) ) ;
#3289 = CARTESIAN_POINT ( 'NONE',  ( 5.939701018627000728, -10.93065061464000109, 320.0000000000000000 ) ) ;
#3290 = ORIENTED_EDGE ( 'NONE', *, *, #5385, .T. ) ;
#3291 = CARTESIAN_POINT ( 'NONE',  ( -0.7231407225213108969, -7.447240517548999961, -434.6679473676751400 ) ) ;
#3292 = AXIS2_PLACEMENT_3D ( 'NONE', #9308, #9094, #4410 ) ;
#3293 = CARTESIAN_POINT ( 'NONE',  ( -16.17578790646000186, -2.500000000000000000, -433.5685902625999688 ) ) ;
#3294 = CARTESIAN_POINT ( 'NONE',  ( 8.717693564518029348, -8.144027366771089405, -314.9999999999999432 ) ) ;
#3295 = ORIENTED_EDGE ( 'NONE', *, *, #8906, .F. ) ;
#3296 = CARTESIAN_POINT ( 'NONE',  ( 17.50000000000107292, 0.7437989020622546299, -314.4963898845653603 ) ) ;
#3297 = ORIENTED_EDGE ( 'NONE', *, *, #10481, .F. ) ;
#3298 = CARTESIAN_POINT ( 'NONE',  ( -18.32558628770999931, 3.116746082530000184, -317.4999999999870397 ) ) ;
#3299 = ORIENTED_EDGE ( 'NONE', *, *, #10436, .F. ) ;
#3300 = CARTESIAN_POINT ( 'NONE',  ( 15.02162735728999543, -8.365494092177003793, -302.9207377450070453 ) ) ;
#3301 = CARTESIAN_POINT ( 'NONE',  ( 18.78102408959999536, -1.459157757289999413, -317.4928077629770087 ) ) ;
#3302 = AXIS2_PLACEMENT_3D ( 'NONE', #9272, #7008, #3568 ) ;
#3303 = VECTOR ( 'NONE', #5234, 1000.000000000000000 ) ;
#3304 = CARTESIAN_POINT ( 'NONE',  ( 15.00000000000326139, -5.136019918588313243E-17, 315.0000000000001137 ) ) ;
#3305 = PRODUCT_DEFINITION ( 'UNKNOWN', '', #6449, #667 ) ;
#3306 =( REPRESENTATION_RELATIONSHIP ('NONE','NONE', #8468, #4020 ) REPRESENTATION_RELATIONSHIP_WITH_TRANSFORMATION ( #6617 )SHAPE_REPRESENTATION_RELATIONSHIP( ) );
#3307 =( NAMED_UNIT ( * ) PLANE_ANGLE_UNIT ( ) SI_UNIT ( $, .RADIAN. ) );
#3308 = CARTESIAN_POINT ( 'NONE',  ( -17.80660862177001746, 5.847896592537999538, -302.9207377450070453 ) ) ;
#3309 = CARTESIAN_POINT ( 'NONE',  ( -46.74071243416547361, -7.500000000000000000, -414.3237589990478114 ) ) ;
#3310 = ORIENTED_EDGE ( 'NONE', *, *, #3941, .T. ) ;
#3311 = CARTESIAN_POINT ( 'NONE',  ( -16.25556153634000367, -3.885850782616000032, -314.4150829855000211 ) ) ;
#3312 = DIRECTION ( 'NONE',  ( 0.000000000000000000, -1.000000000000000000, 0.000000000000000000 ) ) ;
#3313 = AXIS2_PLACEMENT_3D ( 'NONE', #4697, #9693, #2280 ) ;
#3314 = ORIENTED_EDGE ( 'NONE', *, *, #3389, .F. ) ;
#3315 = CARTESIAN_POINT ( 'NONE',  ( -8.858368459239001069, -11.29793033041000250, 190.4207385301700128 ) ) ;
#3316 = CARTESIAN_POINT ( 'NONE',  ( -31.51838671672000558, 2.500000000000000000, -497.7560445212000104 ) ) ;
#3317 = DIRECTION ( 'NONE',  ( -0.000000000000000000, 1.000000000000000000, 0.000000000000000000 ) ) ;
#3318 = FACE_OUTER_BOUND ( 'NONE', #10255, .T. ) ;
#3319 = EDGE_CURVE ( 'NONE', #7492, #8716, #5526, .T. ) ;
#3320 = CARTESIAN_POINT ( 'NONE',  ( 16.21525914616999842, -2.693567875512000054, 315.0848619657999734 ) ) ;
#3321 = EDGE_CURVE ( 'NONE', #1259, #3194, #7259, .T. ) ;
#3322 = CARTESIAN_POINT ( 'NONE',  ( -24.00000000000000000, -2.633704000000000267, -380.4979246178999688 ) ) ;
#3323 = CARTESIAN_POINT ( 'NONE',  ( 8.650961417647998530, -10.84061383582999838, 320.0770942683900557 ) ) ;
#3324 = CARTESIAN_POINT ( 'NONE',  ( 9.075831286667817466, 11.14872141952138840, 319.0000000000005116 ) ) ;
#3325 = CARTESIAN_POINT ( 'NONE',  ( 19.30523607465251956, 3.390426274888739488, -303.4999999999990905 ) ) ;
#3326 = CARTESIAN_POINT ( 'NONE',  ( 16.90887668763000207, -0.2823175147257999673, 315.0848619657999734 ) ) ;
#3327 = ORIENTED_EDGE ( 'NONE', *, *, #8756, .T. ) ;
#3328 = CARTESIAN_POINT ( 'NONE',  ( 4.856005603318365615, -12.14126555804866214, 190.9999999999995737 ) ) ;
#3329 = ORIENTED_EDGE ( 'NONE', *, *, #8250, .F. ) ;
#3330 = VECTOR ( 'NONE', #9820, 1000.000000000000000 ) ;
#3331 = ADVANCED_FACE ( 'NONE', ( #10586 ), #8980, .T. ) ;
#3332 = EDGE_CURVE ( 'NONE', #9806, #1105, #5508, .T. ) ;
#3333 = VECTOR ( 'NONE', #8346, 1000.000000000000000 ) ;
#3334 = CARTESIAN_POINT ( 'NONE',  ( -9.899579175599695802, -4.014440445723298723, -437.8439261505764648 ) ) ;
#3335 = CARTESIAN_POINT ( 'NONE',  ( -19.58578074103510147, 1.999241607805304935E-07, -302.5000071933975505 ) ) ;
#3336 = VECTOR ( 'NONE', #6671, 1000.000000000000000 ) ;
#3337 = CARTESIAN_POINT ( 'NONE',  ( -5.416173751597343156, -12.00000000000000000, -337.7825848737071510 ) ) ;
#3338 = AXIS2_PLACEMENT_3D ( 'NONE', #5821, #679, #1594 ) ;
#3339 = ORIENTED_EDGE ( 'NONE', *, *, #10161, .T. ) ;
#3340 = CARTESIAN_POINT ( 'NONE',  ( 18.32597195921000122, -3.115684853309999891, -302.5000000000129603 ) ) ;
#3341 = AXIS2_PLACEMENT_3D ( 'NONE', #4901, #7324, #975 ) ;
#3342 = SURFACE_STYLE_USAGE ( .BOTH. , #7 ) ;
#3343 = CARTESIAN_POINT ( 'NONE',  ( -46.74071243419621169, -9.500000000000001776, -414.3237589990241077 ) ) ;
#3344 = SURFACE_STYLE_FILL_AREA ( #5700 ) ;
#3345 = DIRECTION ( 'NONE',  ( 0.000000000000000000, -1.000000000000000000, 0.000000000000000000 ) ) ;
#3346 = CARTESIAN_POINT ( 'NONE',  ( 2.381287040813000348E-07, -10.00000001404999850, 190.0000000000000000 ) ) ;
#3347 = CARTESIAN_POINT ( 'NONE',  ( -15.95659996325998087, 7.548489772182000124, -316.3802825947000201 ) ) ;
#3348 = CIRCLE ( 'NONE', #5540, 3.500000000000005773 ) ;
#3349 = AXIS2_PLACEMENT_3D ( 'NONE', #4563, #1993, #7735 ) ;
#3350 = CIRCLE ( 'NONE', #2837, 19.99999999999999289 ) ;
#3351 = ADVANCED_FACE ( 'NONE', ( #3228 ), #8062, .F. ) ;
#3352 = CARTESIAN_POINT ( 'NONE',  ( -15.68033135863999838, -6.468544937636000469, 320.0000000000000000 ) ) ;
#3353 = CARTESIAN_POINT ( 'NONE',  ( -0.3768446329310572995, -7.516309540199999084, -434.3911927895006784 ) ) ;
#3354 = CARTESIAN_POINT ( 'NONE',  ( -2.907097610887497741, -12.50000000000000000, -345.9038247371837542 ) ) ;
#3355 = CARTESIAN_POINT ( 'NONE',  ( 0.7884827272773687890, -9.499887003984508027, -315.0000000000000000 ) ) ;
#3356 = EDGE_LOOP ( 'NONE', ( #1743, #6611, #5222, #3948 ) ) ;
#3357 = CARTESIAN_POINT ( 'NONE',  ( -0.9204674644685997276, -9.999779064329263889, -314.4999424967812729 ) ) ;
#3358 = ORIENTED_EDGE ( 'NONE', *, *, #10436, .T. ) ;
#3359 = CARTESIAN_POINT ( 'NONE',  ( 16.13706688435999581, 6.055114415286000806, -317.5000000000000000 ) ) ;
#3360 = ORIENTED_EDGE ( 'NONE', *, *, #8250, .T. ) ;
#3361 = CARTESIAN_POINT ( 'NONE',  ( -1.983590419337998734, -12.44807596301999908, -303.6197174156509391 ) ) ;
#3362 = STYLED_ITEM ( 'NONE', ( #7988 ), #3778 ) ;
#3363 = CARTESIAN_POINT ( 'NONE',  ( 12.34703828426001770, -8.590819132751997600, -317.4928077629770087 ) ) ;
#3364 = CARTESIAN_POINT ( 'NONE',  ( 14.79012398733999945, -1.483731117707000058, 315.0000000000000000 ) ) ;
#3365 = EDGE_CURVE ( 'NONE', #8331, #4467, #10585, .T. ) ;
#3366 = CARTESIAN_POINT ( 'NONE',  ( -4.143458015209706247, -7.288605749207033746, -435.5329359125040583 ) ) ;
#3367 = CARTESIAN_POINT ( 'NONE',  ( -17.49957620160848393, -0.4465025224747954380, 314.4999504925934275 ) ) ;
#3368 = ORIENTED_EDGE ( 'NONE', *, *, #10050, .F. ) ;
#3369 = CARTESIAN_POINT ( 'NONE',  ( -0.6468861588581515942, -7.500000251058999368, -434.1463208427667269 ) ) ;
#3370 = CARTESIAN_POINT ( 'NONE',  ( 5.145495120689000501, 11.07694361959999974, -302.5000000000000000 ) ) ;
#3371 = VERTEX_POINT ( 'NONE', #5636 ) ;
#3372 = CARTESIAN_POINT ( 'NONE',  ( -13.97596040350999402, -9.042973024665997173, 190.4207385301700128 ) ) ;
#3373 = CARTESIAN_POINT ( 'NONE',  ( -17.50000000000125056, -1.338989683019597976E-14, -315.0000000000000568 ) ) ;
#3374 = CARTESIAN_POINT ( 'NONE',  ( 11.69624556101560664, 6.874206995516638052, -315.0000000000000000 ) ) ;
#3375 = LINE ( 'NONE', #9981, #2567 ) ;
#3376 = CARTESIAN_POINT ( 'NONE',  ( 10.00032506892000406, 10.91649673191999526, 190.4207385301700128 ) ) ;
#3377 = ORIENTED_EDGE ( 'NONE', *, *, #2024, .F. ) ;
#3378 = ORIENTED_EDGE ( 'NONE', *, *, #810, .F. ) ;
#3379 = ADVANCED_FACE ( 'NONE', ( #1620 ), #1669, .T. ) ;
#3380 = DIRECTION ( 'NONE',  ( 0.9554399839384175586, 0.000000000000000000, 0.2951854283188048989 ) ) ;
#3381 = DIRECTION ( 'NONE',  ( 0.000000000000000000, -1.000000000000000000, 0.000000000000000000 ) ) ;
#3382 = CARTESIAN_POINT ( 'NONE',  ( 16.20020866270998638, -5.814836367836996978, 319.9928079742500131 ) ) ;
#3383 = CARTESIAN_POINT ( 'NONE',  ( -17.22665784173602788, 1.821305584325311866, 314.4999396030179355 ) ) ;
#3384 = SURFACE_STYLE_FILL_AREA ( #3491 ) ;
#3385 = CARTESIAN_POINT ( 'NONE',  ( 16.75097866579000083, 2.074182492207000461, 314.8616023057000461 ) ) ;
#3386 = ORIENTED_EDGE ( 'NONE', *, *, #10623, .T. ) ;
#3387 = EDGE_LOOP ( 'NONE', ( #2271, #1201, #9015, #8550 ) ) ;
#3388 = EDGE_CURVE ( 'NONE', #245, #9921, #5795, .T. ) ;
#3389 = EDGE_CURVE ( 'NONE', #9273, #9531, #10402, .T. ) ;
#3390 = CARTESIAN_POINT ( 'NONE',  ( -3.695312159471046076, -2.618857474173998057, -436.9735000885333989 ) ) ;
#3391 = CARTESIAN_POINT ( 'NONE',  ( -8.517242506840645433, 8.210459489885888473, 315.0000000000000568 ) ) ;
#3392 = DIRECTION ( 'NONE',  ( -0.4712473909295827323, 0.000000000000000000, 0.8820010751365675583 ) ) ;
#3393 = EDGE_LOOP ( 'NONE', ( #4194, #2283, #9700, #4269 ) ) ;
#3394 = CARTESIAN_POINT ( 'NONE',  ( -6.503149100579999953, -10.80808940222000025, -302.5000000000000000 ) ) ;
#3395 = SURFACE_STYLE_USAGE ( .BOTH. , #1889 ) ;
#3396 = CARTESIAN_POINT ( 'NONE',  ( -1.762031438543397055, -7.488850308864000382, -434.6217938733590813 ) ) ;
#3397 = ADVANCED_FACE ( 'NONE', ( #3807 ), #7040, .F. ) ;
#3398 = SURFACE_STYLE_USAGE ( .BOTH. , #1729 ) ;
#3399 = CARTESIAN_POINT ( 'NONE',  ( -11.28781796570999951, 4.951468039558000633, -284.9999999999999432 ) ) ;
#3400 = CARTESIAN_POINT ( 'NONE',  ( -51.72607275331812104, -7.500000000000000888, -370.6966883942067739 ) ) ;
#3401 = AXIS2_PLACEMENT_3D ( 'NONE', #5585, #3278, #8170 ) ;
#3402 = CARTESIAN_POINT ( 'NONE',  ( -9.372233899709991434, 11.04684900435999495, -316.3802825947000201 ) ) ;
#3403 = CARTESIAN_POINT ( 'NONE',  ( -38.85901494634669007, -8.000000000000000000, -386.6556615250812570 ) ) ;
#3404 = CARTESIAN_POINT ( 'NONE',  ( 7.462474768419414595, -5.636463904742665676, -525.6703580967167682 ) ) ;
#3405 = DIRECTION ( 'NONE',  ( 0.1283568000945425058, -0.9912279005316182445, 0.03149255590087908507 ) ) ;
#3406 = CARTESIAN_POINT ( 'NONE',  ( 15.52898264372802650, -3.840979768096378866, -315.0000000000000000 ) ) ;
#3407 = ORIENTED_EDGE ( 'NONE', *, *, #9625, .F. ) ;
#3408 = CARTESIAN_POINT ( 'NONE',  ( -17.19853431801041665, 2.231396706186351775, -314.4963898845653603 ) ) ;
#3409 = ORIENTED_EDGE ( 'NONE', *, *, #9957, .T. ) ;
#3410 = CARTESIAN_POINT ( 'NONE',  ( -10.21957842388999893, 9.686567771335999666, -317.5000000000000000 ) ) ;
#3411 = ORIENTED_EDGE ( 'NONE', *, *, #7192, .T. ) ;
#3412 = CARTESIAN_POINT ( 'NONE',  ( 6.532283844592004840, -11.81967986011000704, -303.6197174156509391 ) ) ;
#3413 = CARTESIAN_POINT ( 'NONE',  ( -12.29114107644999443, -8.620527874443991934, -317.4928077629770087 ) ) ;
#3414 = CARTESIAN_POINT ( 'NONE',  ( -16.77957632114000219, 1.244976636274000015, -315.0848619657999734 ) ) ;
#3415 = DIRECTION ( 'NONE',  ( 1.000000000000000000, 0.000000000000000000, 0.000000000000000000 ) ) ;
#3416 = CARTESIAN_POINT ( 'NONE',  ( -15.96001947224000794, 7.545661119572996789, -303.6197174156520759 ) ) ;
#3417 = CARTESIAN_POINT ( 'NONE',  ( -8.993684809926110191, -7.500000000000000888, -419.2513267189134467 ) ) ;
#3418 = EDGE_LOOP ( 'NONE', ( #987, #7447 ) ) ;
#3419 = CARTESIAN_POINT ( 'NONE',  ( -0.5695610819088786636, -7.500000013076999927, -434.2411922114832805 ) ) ;
#3420 = ORIENTED_EDGE ( 'NONE', *, *, #1146, .F. ) ;
#3421 = CARTESIAN_POINT ( 'NONE',  ( 17.00602911426001285, -6.582783228486000837, 191.1197171614399792 ) ) ;
#3422 = CARTESIAN_POINT ( 'NONE',  ( 0.000000000000000000, -10.54711710274999881, -315.0000000000001137 ) ) ;
#3423 = CARTESIAN_POINT ( 'NONE',  ( 16.13978190921854861, 2.966266463780219187, -314.9999999999999432 ) ) ;
#3424 = CARTESIAN_POINT ( 'NONE',  ( -34.37192209820132405, -7.500000000000000000, -461.0868123482146643 ) ) ;
#3425 = CARTESIAN_POINT ( 'NONE',  ( -14.03700484701000484, 9.005201968871000773, 190.4207385301700128 ) ) ;
#3426 = AXIS2_PLACEMENT_3D ( 'NONE', #9072, #43, #9879 ) ;
#3427 = VERTEX_POINT ( 'NONE', #2146 ) ;
#3428 = CARTESIAN_POINT ( 'NONE',  ( 16.10362618234000109, -3.713712614977999760, 314.6383426456000052 ) ) ;
#3429 = DIRECTION ( 'NONE',  ( 0.000000000000000000, 1.000000000000000000, -0.000000000000000000 ) ) ;
#3430 = CARTESIAN_POINT ( 'NONE',  ( -4.863072958136998025, -11.71397411138000422, 320.0770942683900557 ) ) ;
#3431 = CARTESIAN_POINT ( 'NONE',  ( -14.96977070983867009, -8.000000000000000000, -385.2505660326773409 ) ) ;
#3432 = CARTESIAN_POINT ( 'NONE',  ( -98.44423576012317767, -7.500000000000000000, -338.7741350709160315 ) ) ;
#3433 = CARTESIAN_POINT ( 'NONE',  ( 13.31399140613000043, 6.082710156904999721, 314.8616023057000461 ) ) ;
#3434 = ORIENTED_EDGE ( 'NONE', *, *, #9826, .F. ) ;
#3435 = DIRECTION ( 'NONE',  ( -1.000000000000000000, 0.000000000000000000, 0.000000000000000000 ) ) ;
#3436 = ORIENTED_EDGE ( 'NONE', *, *, #9040, .F. ) ;
#3437 = CARTESIAN_POINT ( 'NONE',  ( -14.79708307774000353, 8.514882941861998233, 319.5792614743400009 ) ) ;
#3438 = ORIENTED_EDGE ( 'NONE', *, *, #6940, .F. ) ;
#3439 = AXIS2_PLACEMENT_3D ( 'NONE', #7852, #10078, #2214 ) ;
#3440 = EDGE_CURVE ( 'NONE', #6553, #5580, #10334, .T. ) ;
#3441 = CARTESIAN_POINT ( 'NONE',  ( -5.518773171133347866, -3.002193056125999515, -437.5009914653419401 ) ) ;
#3442 = AXIS2_PLACEMENT_3D ( 'NONE', #5108, #3860, #2036 ) ;
#3443 = CARTESIAN_POINT ( 'NONE',  ( -13.37739799451331457, 5.841934623551301442, 315.0000000000000000 ) ) ;
#3444 = CARTESIAN_POINT ( 'NONE',  ( -1.873948611767810357, -7.500000000000000000, -349.2478646809746579 ) ) ;
#3445 = ORIENTED_EDGE ( 'NONE', *, *, #5099, .T. ) ;
#3446 = ADVANCED_FACE ( 'NONE', ( #6116 ), #5464, .F. ) ;
#3447 = CARTESIAN_POINT ( 'NONE',  ( -0.8444067271132583707, -2.512810845887640809, -434.3277856070802727 ) ) ;
#3448 = FILL_AREA_STYLE ('',( #5208 ) ) ;
#3449 = CARTESIAN_POINT ( 'NONE',  ( -11.92649270223300206, -6.242805967437002224, -437.6501176045007924 ) ) ;
#3450 = PLANE ( 'NONE',  #5140 ) ;
#3451 = DIRECTION ( 'NONE',  ( 0.4712473909295803454, 0.000000000000000000, -0.8820010751365688906 ) ) ;
#3452 = DIRECTION ( 'NONE',  ( -0.6156614753245244209, 0.000000000000000000, 0.7880107536076078611 ) ) ;
#3453 = CARTESIAN_POINT ( 'NONE',  ( -72.90663470102438737, -12.40000000000001101, -375.2168990826883714 ) ) ;
#3454 = DIRECTION ( 'NONE',  ( -0.9712267471052612455, 0.000000000000000000, -0.2381566831044910626 ) ) ;
#3455 = EDGE_CURVE ( 'NONE', #8573, #5049, #1175, .T. ) ;
#3456 = CARTESIAN_POINT ( 'NONE',  ( 7.068287171791554080, -5.589036098012454268, -525.5562187735022235 ) ) ;
#3457 = FACE_OUTER_BOUND ( 'NONE', #6132, .T. ) ;
#3458 = CARTESIAN_POINT ( 'NONE',  ( 11.84501012641003825, -6.794057347756047527, -315.0000000000000000 ) ) ;
#3459 = EDGE_CURVE ( 'NONE', #2618, #5593, #7886, .T. ) ;
#3460 = ORIENTED_EDGE ( 'NONE', *, *, #4238, .F. ) ;
#3461 = DIRECTION ( 'NONE',  ( -0.4824394482813016416, 0.000000000000000000, 0.8759293229148304993 ) ) ;
#3462 = CARTESIAN_POINT ( 'NONE',  ( 3.763664787428660841, -12.29131725939111419, -316.5000000000004547 ) ) ;
#3463 = ORIENTED_EDGE ( 'NONE', *, *, #10535, .F. ) ;
#3464 = DIRECTION ( 'NONE',  ( 0.000000000000000000, 1.000000000000000000, -0.000000000000000000 ) ) ;
#3465 = VERTEX_POINT ( 'NONE', #2039 ) ;
#3466 = CARTESIAN_POINT ( 'NONE',  ( 7.926044316621995378, -11.48136605963999024, -303.6197174156509391 ) ) ;
#3467 = CARTESIAN_POINT ( 'NONE',  ( 11.29610983636999144, -9.103527074753996473, -317.4928077629770087 ) ) ;
#3468 = EDGE_CURVE ( 'NONE', #5957, #2787, #9355, .T. ) ;
#3469 = VECTOR ( 'NONE', #9791, 1000.000000000000114 ) ;
#3470 = DIRECTION ( 'NONE',  ( 0.000000000000000000, 1.000000000000000000, 0.000000000000000000 ) ) ;
#3471 = DIRECTION ( 'NONE',  ( 1.000000000000000000, 0.000000000000000000, 0.000000000000000000 ) ) ;
#3472 = CARTESIAN_POINT ( 'NONE',  ( -7.926044316621995378, 11.48136605963999024, -303.6197174156509391 ) ) ;
#3473 = DIRECTION ( 'NONE',  ( -0.1247904863035891043, 0.000000000000000000, 0.9921831154218023752 ) ) ;
#3474 = EDGE_LOOP ( 'NONE', ( #9966, #5789, #2878, #8887 ) ) ;
#3475 = CARTESIAN_POINT ( 'NONE',  ( -17.34710322845000263, 0.4172063223308000168, -314.6383426456000052 ) ) ;
#3476 = CARTESIAN_POINT ( 'NONE',  ( -6.328188536734999481, 10.84734154703999920, -302.5000000000000000 ) ) ;
#3477 = VERTEX_POINT ( 'NONE', #3649 ) ;
#3478 = AXIS2_PLACEMENT_3D ( 'NONE', #9470, #8549, #8598 ) ;
#3479 = CARTESIAN_POINT ( 'NONE',  ( -6.124940582141004342, -11.99257230354999315, 190.4207385301700128 ) ) ;
#3480 = DIRECTION ( 'NONE',  ( 0.000000000000000000, 0.000000000000000000, -1.000000000000000000 ) ) ;
#3481 = CARTESIAN_POINT ( 'NONE',  ( 13.89455516181870465, 5.448669939092228631, -315.0000000000000000 ) ) ;
#3482 = CARTESIAN_POINT ( 'NONE',  ( 19.21810730420998681, 3.675731523933000400, 190.4207385301700128 ) ) ;
#3483 = CIRCLE ( 'NONE', #6565, 12.50000000000001421 ) ;
#3484 = EDGE_CURVE ( 'NONE', #7857, #199, #8968, .T. ) ;
#3485 = CARTESIAN_POINT ( 'NONE',  ( 16.76545246634000108, -2.037063237379999947, 314.8616023057000461 ) ) ;
#3486 = SURFACE_STYLE_FILL_AREA ( #4292 ) ;
#3487 = CARTESIAN_POINT ( 'NONE',  ( -84.60928256584868734, -2.500000000000000000, -354.0579196189994491 ) ) ;
#3488 = TOROIDAL_SURFACE ( 'NONE', #9326, 15.50000000000000000, 0.5000000000000000000 ) ;
#3489 = CARTESIAN_POINT ( 'NONE',  ( -19.55138120870000407, -0.8505817651195003437, 320.0770942683900557 ) ) ;
#3490 = CARTESIAN_POINT ( 'NONE',  ( -16.56500303248389372, 3.264221055421775652, 314.4999403627584229 ) ) ;
#3491 = FILL_AREA_STYLE ('',( #9831 ) ) ;
#3492 = CARTESIAN_POINT ( 'NONE',  ( 13.56771446467999986, 6.451120369226999607, 314.4150829855000211 ) ) ;
#3493 = ORIENTED_EDGE ( 'NONE', *, *, #3523, .F. ) ;
#3494 = CARTESIAN_POINT ( 'NONE',  ( 19.12881201168725198, -3.682481340332637743, 190.9999999999995737 ) ) ;
#3495 = ORIENTED_EDGE ( 'NONE', *, *, #9062, .F. ) ;
#3496 = CARTESIAN_POINT ( 'NONE',  ( 15.70899585331000559, 7.847162746392004173, 319.5792614743400009 ) ) ;
#3497 = CARTESIAN_POINT ( 'NONE',  ( -1.399570435356993769, -2.031614869683998847, -436.0946480090682940 ) ) ;
#3498 = CARTESIAN_POINT ( 'NONE',  ( 2.545396798794703042, 9.391972178232515844, 315.0000000000000568 ) ) ;
#3499 = ITEM_DEFINED_TRANSFORMATION ( 'NONE', 'NONE', #6104,  #2817 ) ;
#3500 = FACE_OUTER_BOUND ( 'NONE', #10528, .T. ) ;
#3501 = ORIENTED_EDGE ( 'NONE', *, *, #2260, .F. ) ;
#3502 = LINE ( 'NONE', #5050, #5742 ) ;
#3503 = PLANE ( 'NONE',  #929 ) ;
#3504 = CARTESIAN_POINT ( 'NONE',  ( -1.437790087008336881, -7.307863115514998675, -435.8454831066800921 ) ) ;
#3505 = CARTESIAN_POINT ( 'NONE',  ( -53.22217373880035041, -2.500000000000000000, -455.2094346026838139 ) ) ;
#3506 = CARTESIAN_POINT ( 'NONE',  ( -34.37192209818999800, -2.500000000000000000, -461.0868123482000556 ) ) ;
#3507 = CARTESIAN_POINT ( 'NONE',  ( 13.35558048726000635, 8.018799577237007981, 190.0071920248299477 ) ) ;
#3508 = CARTESIAN_POINT ( 'NONE',  ( -8.993684809926110191, -9.000000000000001776, -419.2513267189134467 ) ) ;
#3509 = VECTOR ( 'NONE', #6454, 1000.000000000000000 ) ;
#3510 = PLANE ( 'NONE',  #6133 ) ;
#3511 = CARTESIAN_POINT ( 'NONE',  ( -1.999999999997229772, -2.500000000000000000, -409.4999999999571969 ) ) ;
#3512 = CARTESIAN_POINT ( 'NONE',  ( -46.74071243419621169, -9.000000000000001776, -414.3237589990241077 ) ) ;
#3513 = CARTESIAN_POINT ( 'NONE',  ( -10.02545106797885310, -7.672278800222116502, -315.0000000000000000 ) ) ;
#3514 = ORIENTED_EDGE ( 'NONE', *, *, #8088, .F. ) ;
#3515 = DIRECTION ( 'NONE',  ( 0.4712473909295827323, 0.000000000000000000, -0.8820010751365675583 ) ) ;
#3516 = CARTESIAN_POINT ( 'NONE',  ( -4.978134047761750836, -12.12024670600909459, -316.5000000000004547 ) ) ;
#3517 = ORIENTED_EDGE ( 'NONE', *, *, #6082, .F. ) ;
#3518 = PLANE ( 'NONE',  #8100 ) ;
#3519 = EDGE_LOOP ( 'NONE', ( #7980, #7700, #4109, #4658 ) ) ;
#3520 = VECTOR ( 'NONE', #3211, 1000.000000000000000 ) ;
#3521 = AXIS2_PLACEMENT_3D ( 'NONE', #8895, #1644, #9916 ) ;
#3522 = CARTESIAN_POINT ( 'NONE',  ( -13.35621109890998959, 8.022534180767001644, -317.4928077629770087 ) ) ;
#3523 = EDGE_CURVE ( 'NONE', #9383, #4786, #6703, .T. ) ;
#3524 = CIRCLE ( 'NONE', #1458, 3.499999999999999112 ) ;
#3525 = CARTESIAN_POINT ( 'NONE',  ( 12.67153153313999070, -9.210367834107003659, -317.5770954168139610 ) ) ;
#3526 = CARTESIAN_POINT ( 'NONE',  ( -16.60805916514000202, 2.908391789136000050, -314.6383426456000052 ) ) ;
#3527 = CARTESIAN_POINT ( 'NONE',  ( -6.532283844592004840, 11.81967986011000704, -303.6197174156520759 ) ) ;
#3528 = CARTESIAN_POINT ( 'NONE',  ( 9.526067998327799539E-10, -10.00000000005854339, 314.4999528359535361 ) ) ;
#3529 = ORIENTED_EDGE ( 'NONE', *, *, #8365, .F. ) ;
#3530 = CARTESIAN_POINT ( 'NONE',  ( 18.78737820286000115, -1.762683282930000095, 190.0000000000000000 ) ) ;
#3531 = CARTESIAN_POINT ( 'NONE',  ( -7.649658656166000270, 10.52693506402999901, -302.5000000000000000 ) ) ;
#3532 = ORIENTED_EDGE ( 'NONE', *, *, #8111, .T. ) ;
#3533 = CARTESIAN_POINT ( 'NONE',  ( 20.08953225942999765, -0.1031351683529000418, 190.4207385301700128 ) ) ;
#3534 = DIRECTION ( 'NONE',  ( 0.000000000000000000, 1.000000000000000000, 0.000000000000000000 ) ) ;
#3535 = CARTESIAN_POINT ( 'NONE',  ( 16.88803284296001905, -5.077274453104001495, -302.5071922382879279 ) ) ;
#3536 = EDGE_CURVE ( 'NONE', #6553, #168, #9721, .T. ) ;
#3537 = CARTESIAN_POINT ( 'NONE',  ( -18.68134283559999531, 4.475435185431997809, 191.1197171614399792 ) ) ;
#3538 = COLOUR_RGB ( '', 0.09019608, 0.27058824, 0.51372549) ;
#3539 = ORIENTED_EDGE ( 'NONE', *, *, #7327, .F. ) ;
#3540 = CARTESIAN_POINT ( 'NONE',  ( 10.49789511286000021, -7.639556387670999982, 314.8616023057000461 ) ) ;
#3541 = DIRECTION ( 'NONE',  ( 0.7426245373610016465, 0.000000000000000000, -0.6697079934638365817 ) ) ;
#3542 = CARTESIAN_POINT ( 'NONE',  ( 12.02088824526999211, -10.08549396686999522, 319.5792614743400009 ) ) ;
#3543 = CARTESIAN_POINT ( 'NONE',  ( -11.54108038788630708, 7.525558202395652430, 314.4999425153563948 ) ) ;
#3544 = CARTESIAN_POINT ( 'NONE',  ( -19.99999035944999903, 7.277427703818000446E-10, -303.5000000000000000 ) ) ;
#3545 = CARTESIAN_POINT ( 'NONE',  ( 17.12450099635000100, -0.4005340032738999856, 314.8616023057000461 ) ) ;
#3546 = EDGE_LOOP ( 'NONE', ( #1905, #1773, #10, #788 ) ) ;
#3547 = CARTESIAN_POINT ( 'NONE',  ( -78.61675616006050404, -2.500000000000000000, -344.0534392588842252 ) ) ;
#3548 = CARTESIAN_POINT ( 'NONE',  ( -4.404324556173000005, 12.28809208595000335, 319.5792614743400009 ) ) ;
#3549 = AXIS2_PLACEMENT_3D ( 'NONE', #5370, #2104, #10320 ) ;
#3550 = CARTESIAN_POINT ( 'NONE',  ( 10.00000000000000000, 2.500000000000000000, -272.5000000000000000 ) ) ;
#3551 = CARTESIAN_POINT ( 'NONE',  ( 4.648656036509398959, 9.134414902114890822, 315.0000000000000568 ) ) ;
#3552 = DIRECTION ( 'NONE',  ( -0.000000000000000000, 1.000000000000000000, 0.000000000000000000 ) ) ;
#3553 = VERTEX_POINT ( 'NONE', #5734 ) ;
#3554 = CARTESIAN_POINT ( 'NONE',  ( -9.006891093149000938, -10.12158591819999920, -302.5000000000000000 ) ) ;
#3555 = CIRCLE ( 'NONE', #1666, 3.500000000000003109 ) ;
#3556 = CARTESIAN_POINT ( 'NONE',  ( 8.548650239411999863, 10.26553531915999962, 190.0000000000000000 ) ) ;
#3557 = CARTESIAN_POINT ( 'NONE',  ( -16.99996037728000076, 1.352916535802999941E-09, -314.9999801883000146 ) ) ;
#3558 = CARTESIAN_POINT ( 'NONE',  ( -18.86316454545999832, -0.4769905026584997931, 190.0071920248299477 ) ) ;
#3559 = FACE_OUTER_BOUND ( 'NONE', #3209, .T. ) ;
#3560 = DIRECTION ( 'NONE',  ( 0.000000000000000000, -1.000000000000000000, 0.000000000000000000 ) ) ;
#3561 = CARTESIAN_POINT ( 'NONE',  ( 8.920203998736104367, -5.829398780986294604, -525.5186553700950753 ) ) ;
#3562 = FACE_OUTER_BOUND ( 'NONE', #9580, .T. ) ;
#3563 = ORIENTED_EDGE ( 'NONE', *, *, #4591, .F. ) ;
#3564 = AXIS2_PLACEMENT_3D ( 'NONE', #8918, #5528, #5635 ) ;
#3565 = CARTESIAN_POINT ( 'NONE',  ( 14.96969266857001557, 6.905075921034003805, 319.9928079742500131 ) ) ;
#3566 = CARTESIAN_POINT ( 'NONE',  ( -15.92495094281444601, -7.583842622554347379, -316.5000000000004547 ) ) ;
#3567 = ORIENTED_EDGE ( 'NONE', *, *, #7921, .T. ) ;
#3568 = DIRECTION ( 'NONE',  ( 0.000000000000000000, 0.000000000000000000, -1.000000000000000000 ) ) ;
#3569 = ORIENTED_EDGE ( 'NONE', *, *, #1096, .F. ) ;
#3570 = CARTESIAN_POINT ( 'NONE',  ( -6.508337484872001255, 10.68452134396000375, -317.4928077629770087 ) ) ;
#3571 = ADVANCED_FACE ( 'NONE', ( #4883 ), #6381, .F. ) ;
#3572 = CARTESIAN_POINT ( 'NONE',  ( -7.885457619219000236, -11.57957576882999184, -317.0792622552969533 ) ) ;
#3573 = CARTESIAN_POINT ( 'NONE',  ( -72.90663470102438737, -12.50000000000000000, -371.7168990826883714 ) ) ;
#3574 = VECTOR ( 'NONE', #4453, 1000.000000000000000 ) ;
#3575 = ADVANCED_FACE ( 'NONE', ( #8209 ), #8789, .T. ) ;
#3576 = LINE ( 'NONE', #7068, #7433 ) ;
#3577 = CARTESIAN_POINT ( 'NONE',  ( 10.19111349739211292, -9.999999999041103038, 314.9999999999999432 ) ) ;
#3578 = ORIENTED_EDGE ( 'NONE', *, *, #1096, .T. ) ;
#3579 = CARTESIAN_POINT ( 'NONE',  ( -12.50247260085999912, -8.641513563414997989, 190.0000000000000000 ) ) ;
#3580 = EDGE_CURVE ( 'NONE', #9479, #514, #10411, .T. ) ;
#3581 = CARTESIAN_POINT ( 'NONE',  ( -24.51838671671999847, -2.500000000000000000, -497.7560445212000104 ) ) ;
#3582 = VERTEX_POINT ( 'NONE', #1554 ) ;
#3583 = DIRECTION ( 'NONE',  ( 9.254477013072932692E-13, 1.000000000000000000, 9.977795243863814969E-14 ) ) ;
#3584 = ORIENTED_EDGE ( 'NONE', *, *, #3700, .F. ) ;
#3585 = CARTESIAN_POINT ( 'NONE',  ( -16.53777229716873265, -2.187293290751350483, 315.0000000000000000 ) ) ;
#3586 = CARTESIAN_POINT ( 'NONE',  ( -18.77308876972001173, -1.495304374661000413, -302.5071922382879279 ) ) ;
#3587 = CARTESIAN_POINT ( 'NONE',  ( 20.08919666923998903, 0.07462331497654001167, 190.4207385301700128 ) ) ;
#3588 = DIRECTION ( 'NONE',  ( 0.000000000000000000, -1.000000000000000000, 0.000000000000000000 ) ) ;
#3589 = ADVANCED_FACE ( 'NONE', ( #10517 ), #696, .T. ) ;
#3590 = CARTESIAN_POINT ( 'NONE',  ( 18.18877801098002323, 4.514014122889999037, -302.4229045757450081 ) ) ;
#3591 = CARTESIAN_POINT ( 'NONE',  ( -1.330908921489000418, -12.56946842516999041, 319.5792614743400009 ) ) ;
#3592 = CARTESIAN_POINT ( 'NONE',  ( 16.97404422732000029, -2.118410180888999683, -314.6383426456000052 ) ) ;
#3593 = CARTESIAN_POINT ( 'NONE',  ( -8.759386130138000937, 8.782224002452998946, 314.4150829855000211 ) ) ;
#3594 = ORIENTED_EDGE ( 'NONE', *, *, #1338, .F. ) ;
#3595 = CARTESIAN_POINT ( 'NONE',  ( 11.67891759455000056, -8.922363378240000031, 190.0071920248299477 ) ) ;
#3596 = ORIENTED_EDGE ( 'NONE', *, *, #6260, .F. ) ;
#3597 = CARTESIAN_POINT ( 'NONE',  ( 18.70581557644998938, 4.435354026251000725, 318.8802828394900644 ) ) ;
#3598 =( BOUNDED_SURFACE ( )  B_SPLINE_SURFACE ( 3, 1, ( 
 ( #4942, #3876 ),
 ( #3227, #1455 ),
 ( #7153, #7260 ),
 ( #10424, #6504 ),
 ( #3064, #8869 ),
 ( #9784, #2423 ),
 ( #3116, #4738 ) ),
 .UNSPECIFIED., .F., .F., .T. ) 
 B_SPLINE_SURFACE_WITH_KNOTS ( ( 4, 3, 4 ),
 ( 2, 2 ),
 ( 0.000000000000000000, 0.5000000000000000000, 1.000000000000000000 ),
 ( 0.000000000000000000, 1.000000000000000000 ),
 .UNSPECIFIED. ) 
 GEOMETRIC_REPRESENTATION_ITEM ( )  RATIONAL_B_SPLINE_SURFACE ( (
 ( 1.000000000000000000, 1.000000000000000000),
 ( 0.8047378540737379904, 0.8047378540737379904),
 ( 0.8047378540737379904, 0.8047378540737379904),
 ( 1.000000000000000000, 1.000000000000000000),
 ( 0.8047378540737379904, 0.8047378540737379904),
 ( 0.8047378540737379904, 0.8047378540737379904),
 ( 1.000000000000000000, 1.000000000000000000) ) ) 
 REPRESENTATION_ITEM ( '' )  SURFACE ( )  );
#3599 = TOROIDAL_SURFACE ( 'NONE', #6328, 12.00000000000000000, 0.5000000000000000000 ) ;
#3600 = VECTOR ( 'NONE', #5647, 1000.000000000000000 ) ;
#3601 = LINE ( 'NONE', #6883, #3909 ) ;
#3602 = CARTESIAN_POINT ( 'NONE',  ( 8.717521301463110106, 8.144085127293724469, 314.9999999999999432 ) ) ;
#3603 = CARTESIAN_POINT ( 'NONE',  ( 11.71572875238734213, -12.50000000010304113, 319.0000000000000568 ) ) ;
#3604 = AXIS2_PLACEMENT_3D ( 'NONE', #4267, #9317, #9103 ) ;
#3605 = CARTESIAN_POINT ( 'NONE',  ( -0.5534908175310586653, -2.500000333914000006, -434.2941325283891274 ) ) ;
#3606 = DIRECTION ( 'NONE',  ( 0.000000000000000000, 1.000000000000000000, -0.000000000000000000 ) ) ;
#3607 = CARTESIAN_POINT ( 'NONE',  ( 15.64479012893000132, 6.500532800106000764, 190.0000000000000000 ) ) ;
#3608 = CARTESIAN_POINT ( 'NONE',  ( 19.38368284813939013, -2.500000000000000000, -515.5999187775453265 ) ) ;
#3609 = CARTESIAN_POINT ( 'NONE',  ( -13.41272981818000432, 7.983430642947998201, 190.0071920248299477 ) ) ;
#3610 = DIRECTION ( 'NONE',  ( 0.000000000000000000, 0.000000000000000000, -1.000000000000000000 ) ) ;
#3611 = AXIS2_PLACEMENT_3D ( 'NONE', #5020, #7500, #4066 ) ;
#3612 = CARTESIAN_POINT ( 'NONE',  ( 8.669822292802292552, -4.205922955401560692, -525.6304339756592299 ) ) ;
#3613 = CARTESIAN_POINT ( 'NONE',  ( 7.445183927592051276, -5.634377803598318302, -525.6654729546380622 ) ) ;
#3614 = EDGE_CURVE ( 'NONE', #3427, #1407, #1068, .T. ) ;
#3615 = CARTESIAN_POINT ( 'NONE',  ( 11.72570362167166635, -6.858483604278664103, 315.0000000000000000 ) ) ;
#3616 = CARTESIAN_POINT ( 'NONE',  ( -4.061138133959000029, 9.851562218542998295, -314.4150829855000211 ) ) ;
#3617 = B_SPLINE_CURVE_WITH_KNOTS ( 'NONE', 3,
 ( #669, #1524, #4806, #8079, #721, #130, #5007, #1636, #1737, #7489, #4104, #1846, #8394, #9104, #3406, #7384, #1792, #6740, #4910, #8188, #2441, #5711, #8996, #6575, #8234, #872, #4320, #8286, #925, #10014, #5810, #19, #2602, #3458, #7538, #7436, #6521, #9155, #6681, #2655, #5923, #825, #9803, #3294, #9050, #4213, #5063, #9960, #1032, #9214, #5117, #5761, #10602, #185, #5863, #1686, #8343, #9857, #2496, #4960, #4158, #73, #6631, #3355, #981, #9908, #3244, #2546, #4268, #1284, #10413, #2251, #589, #7590, #8689, #9558, #3752, #8581, #3055, #2197, #4613, #7888, #5466, #8745, #4505, #239, #1227, #5413, #1387, #3513, #484, #4671, #7043, #9454, #6990, #2041, #10261, #8637, #6935, #3868, #7782, #6323, #10312, #4562, #535, #3809, #2949, #2149, #7097, #2092, #9406, #10213, #6222, #7946, #9612, #7835, #5309, #7145, #9507, #428, #3705, #2898, #5519, #1334, #10362, #3004 ),
 .UNSPECIFIED., .F., .F.,
 ( 4, 1, 1, 1, 1, 1, 2, 2, 1, 1, 1, 1, 1, 2, 2, 1, 1, 1, 1, 1, 2, 2, 1, 1, 1, 1, 1, 2, 2, 1, 1, 1, 1, 1, 1, 2, 2, 1, 1, 1, 1, 1, 2, 2, 1, 1, 2, 2, 2, 1, 1, 2, 2, 1, 1, 1, 1, 2, 2, 1, 1, 1, 1, 1, 1, 2, 2, 1, 1, 1, 1, 1, 2, 2, 1, 1, 1, 1, 1, 2, 2, 1, 1, 1, 1, 1, 2, 2, 1, 1, 1, 1, 2, 2, 4 ),
 ( 0.000000000000000000, 0.06250000000000707767, 0.09375000000001063039, 0.1093750000000124206, 0.1171875000000132255, 0.1210937500000135308, 0.1230468750000135864, 0.1250000000000136280, 0.1562500000000150158, 0.1718750000000157374, 0.1796875000000160982, 0.1835937500000163480, 0.1855468750000164591, 0.1865234375000165423, 0.1875000000000166256, 0.2187500000000192069, 0.2343750000000205669, 0.2421875000000212608, 0.2460937500000216493, 0.2480468750000218991, 0.2490234375000220102, 0.2500000000000220934, 0.2812500000000249245, 0.2968750000000263678, 0.3046875000000271450, 0.3085937500000274780, 0.3105468750000275890, 0.3115234375000275890, 0.3125000000000275335, 0.3437500000000278666, 0.3593750000000280886, 0.3671875000000281997, 0.3710937500000282552, 0.3730468750000283107, 0.3740234375000284217, 0.3745117187500284217, 0.3750000000000284217, 0.4062500000000292544, 0.4218750000000296985, 0.4296875000000299205, 0.4335937500000300315, 0.4355468750000300870, 0.4365234375000300870, 0.4375000000000300315, 0.4531250000000301426, 0.4609375000000301981, 0.4648437500000302536, 0.4687500000000303091, 0.5000000000000306422, 0.5156250000000307532, 0.5234375000000308642, 0.5273437500000308642, 0.5312500000000308642, 0.5468750000000310862, 0.5546875000000311973, 0.5585937500000311973, 0.5605468750000311973, 0.5615234375000311973, 0.5625000000000311973, 0.5937500000000296430, 0.6093750000000288658, 0.6171875000000285327, 0.6210937500000284217, 0.6230468750000283107, 0.6240234375000283107, 0.6245117187500283107, 0.6250000000000283107, 0.6562500000000291989, 0.6718750000000295319, 0.6796875000000297540, 0.6835937500000298650, 0.6855468750000299760, 0.6865234375000299760, 0.6875000000000299760, 0.7187500000000309752, 0.7343750000000314193, 0.7421875000000316414, 0.7460937500000317524, 0.7480468750000318634, 0.7490234375000318634, 0.7500000000000318634, 0.7812500000000318634, 0.7968750000000317524, 0.8046875000000317524, 0.8085937500000317524, 0.8105468750000316414, 0.8115234375000315303, 0.8125000000000314193, 0.8437500000000285327, 0.8593750000000272005, 0.8671875000000265343, 0.8710937500000260902, 0.8730468750000258682, 0.8750000000000255351, 1.000000000000000000 ),
 .UNSPECIFIED. ) ;
#3618 = ORIENTED_EDGE ( 'NONE', *, *, #4169, .F. ) ;
#3619 = CARTESIAN_POINT ( 'NONE',  ( -4.237945188771000460, 11.10223611999999704, 319.9928079742500131 ) ) ;
#3620 = VECTOR ( 'NONE', #9401, 1000.000000000000000 ) ;
#3621 = CARTESIAN_POINT ( 'NONE',  ( -19.86381236214655033, -1.775476277371077716, -316.5000000000004547 ) ) ;
#3622 = CARTESIAN_POINT ( 'NONE',  ( -2.000000000003786749, -9.500000000000001776, -409.4999999999758415 ) ) ;
#3623 = ORIENTED_EDGE ( 'NONE', *, *, #1940, .T. ) ;
#3624 = CARTESIAN_POINT ( 'NONE',  ( 4.800908653447998553, 11.01413625319999845, -317.4928077629770087 ) ) ;
#3625 = CARTESIAN_POINT ( 'NONE',  ( 19.95938911887002831, -1.720557998077001827, -317.0792622552969533 ) ) ;
#3626 = CARTESIAN_POINT ( 'NONE',  ( -36.01445213885307339, -7.656480000000000175, -460.8005622778243264 ) ) ;
#3627 = CARTESIAN_POINT ( 'NONE',  ( 10.00000000000000000, -2.500000000000000000, -285.0000000000000000 ) ) ;
#3628 = CIRCLE ( 'NONE', #1392, 12.50000000000001243 ) ;
#3629 = ORIENTED_EDGE ( 'NONE', *, *, #4360, .F. ) ;
#3630 = CARTESIAN_POINT ( 'NONE',  ( 14.24871951745999965, -7.583581010724000038, 190.0000000000000000 ) ) ;
#3631 = DIRECTION ( 'NONE',  ( 0.000000000000000000, -1.000000000000000000, 0.000000000000000000 ) ) ;
#3632 = EDGE_LOOP ( 'NONE', ( #8374, #2338, #2021, #4086 ) ) ;
#3633 = CYLINDRICAL_SURFACE ( 'NONE', #6556, 2.000000000000033307 ) ;
#3634 = VERTEX_POINT ( 'NONE', #1005 ) ;
#3635 = CARTESIAN_POINT ( 'NONE',  ( -56.92031869107000119, 2.500000000000000000, -403.1217184488000385 ) ) ;
#3636 = CARTESIAN_POINT ( 'NONE',  ( -28.01838671672410896, -7.500000000000000000, -497.7560445212019999 ) ) ;
#3637 = CARTESIAN_POINT ( 'NONE',  ( 12.03935733796000562, 9.983683518723006856, 191.1197171614399792 ) ) ;
#3638 = CARTESIAN_POINT ( 'NONE',  ( -19.99999721801999897, -7.771324026006999692E-11, 191.0000000000000000 ) ) ;
#3639 = DIRECTION ( 'NONE',  ( 0.9396926207858972147, 0.000000000000000000, 0.3420201433256990775 ) ) ;
#3640 = CARTESIAN_POINT ( 'NONE',  ( 19.85665319583999988, -1.941121513171000901, 319.5792614743400009 ) ) ;
#3641 = VECTOR ( 'NONE', #4192, 1000.000000000000227 ) ;
#3642 = CARTESIAN_POINT ( 'NONE',  ( 16.92217352393999974, -0.01966449385449000123, -315.0848619657999734 ) ) ;
#3643 = CARTESIAN_POINT ( 'NONE',  ( -4.031301020048999817, 9.630010295875997883, 314.6383426456000052 ) ) ;
#3644 = ORIENTED_EDGE ( 'NONE', *, *, #4033, .T. ) ;
#3645 = CARTESIAN_POINT ( 'NONE',  ( 6.173727351415999820, -10.75865019063000183, 190.0071920248299477 ) ) ;
#3646 = CARTESIAN_POINT ( 'NONE',  ( -0.6590269763235730993, -7.499720857620891579, -434.1629514920128372 ) ) ;
#3647 = CIRCLE ( 'NONE', #9146, 3.499999999999999556 ) ;
#3648 = DIRECTION ( 'NONE',  ( 0.000000000000000000, -1.000000000000000000, 0.000000000000000000 ) ) ;
#3649 = CARTESIAN_POINT ( 'NONE',  ( -20.40121062015000319, 2.500000000000000000, -430.0210166885000262 ) ) ;
#3650 = CARTESIAN_POINT ( 'NONE',  ( 20.00000000000000000, 0.000000000000000000, 191.0000000000000000 ) ) ;
#3651 = CARTESIAN_POINT ( 'NONE',  ( -14.37110465573396212, -2.500000000000000000, -348.9812360766022721 ) ) ;
#3652 = DIRECTION ( 'NONE',  ( 0.9902680687415800209, 0.000000000000000000, 0.1391731009599966873 ) ) ;
#3653 = CARTESIAN_POINT ( 'NONE',  ( -9.749126195418856611, -6.234330207147000813, -438.4907298204056474 ) ) ;
#3654 = EDGE_CURVE ( 'NONE', #1489, #3077, #3483, .T. ) ;
#3655 = CARTESIAN_POINT ( 'NONE',  ( -16.99964540243389521, 0.4333634660859943533, -315.0000000000000568 ) ) ;
#3656 = CARTESIAN_POINT ( 'NONE',  ( -6.173727351415999820, 10.75865019063000183, 190.0071920248299477 ) ) ;
#3657 = DIRECTION ( 'NONE',  ( 1.000000000000000000, 0.000000000000000000, 0.000000000000000000 ) ) ;
#3658 = ADVANCED_FACE ( 'NONE', ( #8419 ), #8261, .T. ) ;
#3659 = LINE ( 'NONE', #5476, #4420 ) ;
#3660 = DIRECTION ( 'NONE',  ( -0.000000000000000000, 1.000000000000000000, 0.000000000000000000 ) ) ;
#3661 = CARTESIAN_POINT ( 'NONE',  ( 11.54746845216141082, -6.952771041492575854, 315.0000000000000000 ) ) ;
#3662 = CARTESIAN_POINT ( 'NONE',  ( -14.43094748301999886, 5.211771040651000497, -314.8616023057000461 ) ) ;
#3663 = ORIENTED_EDGE ( 'NONE', *, *, #8809, .F. ) ;
#3664 = CARTESIAN_POINT ( 'NONE',  ( -13.31009360926000085, 8.046300872832002682, 319.9928079742500131 ) ) ;
#3665 = DIRECTION ( 'NONE',  ( 0.4712473909295827323, 0.000000000000000000, -0.8820010751365675583 ) ) ;
#3666 = ORIENTED_EDGE ( 'NONE', *, *, #5598, .T. ) ;
#3667 = DIRECTION ( 'NONE',  ( 0.1119865428368791299, 0.000000000000000000, -0.9937097233213750824 ) ) ;
#3668 = CARTESIAN_POINT ( 'NONE',  ( -16.90418428017002839, -6.814536637555997700, -317.0792622552969533 ) ) ;
#3669 = ADVANCED_FACE ( 'NONE', ( #9075 ), #4344, .T. ) ;
#3670 = AXIS2_PLACEMENT_3D ( 'NONE', #8121, #6401, #758 ) ;
#3671 =( BOUNDED_SURFACE ( )  B_SPLINE_SURFACE ( 3, 3, ( 
 ( #3558, #1893, #9459, #1180, #10220, #10267, #8491, #4413, #1133, #7688, #7637, #332, #6839, #8643, #3609, #7584, #6892, #7739, #10159, #383, #9261, #3656, #6942, #6996, #2802, #6074, #2855, #6123, #9364, #1998, #5164, #5263, #231, #9411, #10108, #3507, #2046, #5314, #8587, #6019, #10061, #1234, #434, #2904, #5969, #8437, #4364, #2750, #9313, #10316 ),
 ( #1451, #3815, #2204, #489, #8057, #5418, #6390, #4678, #649, #9670, #7101, #4568, #3974, #4736, #8008, #4788, #3009, #7257, #1289, #5634, #10420, #10368, #702, #6284, #7842, #3925, #5524, #2369, #2313, #9513, #10526, #3172, #5582, #3757, #7048, #8806, #9564, #7204, #598, #8694, #9728, #2956, #1507, #10472, #1340, #6227, #2154, #4621, #3114, #7893 ),
 ( #540, #5474, #8751, #1394, #7952, #3874, #6332, #3061, #7151, #8865, #6446, #9617, #2257, #6815, #3425, #7613, #6705, #896, #7509, #5833, #8364, #1708, #9288, #7669, #1001, #4182, #10087, #6653, #10036, #310, #5887, #3376, #2728, #1868, #151, #1920, #8416, #4235, #7455, #4394, #4289, #7561, #206, #3482, #9236, #1819, #8465, #3587, #5192, #9181 ),
 ( #5084, #6867, #6763, #2680, #5949, #9930, #1108, #3537, #5137, #1056, #4340, #5996, #261, #9126, #4981, #2566, #10136, #8258, #2777, #8916, #99, #1761, #9982, #8311, #5031, #2624, #951, #8564, #9339, #2127, #10297, #7128, #3791, #3637, #9540, #2180, #10345, #10395, #1161, #2934, #1210, #6201, #5338, #2834, #3846, #8519, #6259, #9487, #6103, #6048 ) ),
 .UNSPECIFIED., .F., .F., .T. ) 
 B_SPLINE_SURFACE_WITH_KNOTS ( ( 4, 4 ),
 ( 4, 1, 1, 1, 1, 1, 1, 1, 1, 1, 1, 1, 1, 1, 1, 1, 1, 1, 1, 1, 1, 1, 1, 1, 1, 1, 1, 1, 1, 1, 1, 1, 1, 1, 1, 1, 1, 1, 1, 1, 1, 1, 1, 1, 1, 1, 1, 4 ),
 ( 0.000000000000000000, 1.000000000000000000 ),
 ( -0.008478179454678999930, 0.000000000000000000, 0.01942502340896999982, 0.03767429839031000149, 0.05516856733836000143, 0.07225070737889999206, 0.08921661857028999332, 0.1062419522249000020, 0.1231986756591000043, 0.1401197909732000146, 0.1574955775699000138, 0.1756558812635999889, 0.1944176066207999876, 0.2136589569993999904, 0.2335613621991999844, 0.2542018781120999882, 0.2753083038155999529, 0.2968879296931000167, 0.3196642413612000300, 0.3444503751709999673, 0.3720414184181000117, 0.4028839481288000179, 0.4370422198952000348, 0.4744802605176999810, 0.5138140658555000462, 0.5525504936030000147, 0.5886556970966999591, 0.6214671571023999697, 0.6505675624772999655, 0.6761140898808000177, 0.6991730762615999684, 0.7208971548058999979, 0.7423774111579999335, 0.7637103432859999597, 0.7842694365818000390, 0.8040102150915000578, 0.8232128915810998926, 0.8418292181656999995, 0.8596651317910000145, 0.8769212066234000069, 0.8939598742608000359, 0.9109129999441000214, 0.9278339763510999871, 0.9449158864711000305, 0.9624195949295000219, 0.9806529035300000086, 1.000000000000000000, 1.007725586608000157 ),
 .UNSPECIFIED. ) 
 GEOMETRIC_REPRESENTATION_ITEM ( )  RATIONAL_B_SPLINE_SURFACE ( (
 ( 1.236576749365999817, 1.236576749365999817, 1.236576749365999817, 1.236576749365999817, 1.236576749365999817, 1.236576749365999817, 1.236576749365999817, 1.236576749365999817, 1.236576749365999817, 1.236576749365999817, 1.236576749365999817, 1.236576749365999817, 1.236576749365999817, 1.236576749365999817, 1.236576749365999817, 1.236576749365999817, 1.236576749365999817, 1.236576749365999817, 1.236576749365999817, 1.236576749365999817, 1.236576749365999817, 1.236576749365999817, 1.236576749365999817, 1.236576749365999817, 1.236576749365999817, 1.236576749365999817, 1.236576749365999817, 1.236576749365999817, 1.236576749365999817, 1.236576749365999817, 1.236576749365999817, 1.236576749365999817, 1.236576749365999817, 1.236576749365999817, 1.236576749365999817, 1.236576749365999817, 1.236576749365999817, 1.236576749365999817, 1.236576749365999817, 1.236576749365999817, 1.236576749365999817, 1.236576749365999817, 1.236576749365999817, 1.236576749365999817, 1.236576749365999817, 1.236576749365999817, 1.236576749365999817, 1.236576749365999817, 1.236576749365999817, 1.236576749365999817),
 ( 0.9211410835446999235, 0.9211410835446999235, 0.9211410835446999235, 0.9211410835446999235, 0.9211410835446999235, 0.9211410835446999235, 0.9211410835446999235, 0.9211410835446999235, 0.9211410835446999235, 0.9211410835446999235, 0.9211410835446999235, 0.9211410835446999235, 0.9211410835446999235, 0.9211410835446999235, 0.9211410835446999235, 0.9211410835446999235, 0.9211410835446999235, 0.9211410835446999235, 0.9211410835446999235, 0.9211410835446999235, 0.9211410835446999235, 0.9211410835446999235, 0.9211410835446999235, 0.9211410835446999235, 0.9211410835446999235, 0.9211410835446999235, 0.9211410835446999235, 0.9211410835446999235, 0.9211410835446999235, 0.9211410835446999235, 0.9211410835446999235, 0.9211410835446999235, 0.9211410835446999235, 0.9211410835446999235, 0.9211410835446999235, 0.9211410835446999235, 0.9211410835446999235, 0.9211410835446999235, 0.9211410835446999235, 0.9211410835446999235, 0.9211410835446999235, 0.9211410835446999235, 0.9211410835446999235, 0.9211410835446999235, 0.9211410835446999235, 0.9211410835446999235, 0.9211410835446999235, 0.9211410835446999235, 0.9211410835446999235, 0.9211410835446999235),
 ( 0.9211410835446999235, 0.9211410835446999235, 0.9211410835446999235, 0.9211410835446999235, 0.9211410835446999235, 0.9211410835446999235, 0.9211410835446999235, 0.9211410835446999235, 0.9211410835446999235, 0.9211410835446999235, 0.9211410835446999235, 0.9211410835446999235, 0.9211410835446999235, 0.9211410835446999235, 0.9211410835446999235, 0.9211410835446999235, 0.9211410835446999235, 0.9211410835446999235, 0.9211410835446999235, 0.9211410835446999235, 0.9211410835446999235, 0.9211410835446999235, 0.9211410835446999235, 0.9211410835446999235, 0.9211410835446999235, 0.9211410835446999235, 0.9211410835446999235, 0.9211410835446999235, 0.9211410835446999235, 0.9211410835446999235, 0.9211410835446999235, 0.9211410835446999235, 0.9211410835446999235, 0.9211410835446999235, 0.9211410835446999235, 0.9211410835446999235, 0.9211410835446999235, 0.9211410835446999235, 0.9211410835446999235, 0.9211410835446999235, 0.9211410835446999235, 0.9211410835446999235, 0.9211410835446999235, 0.9211410835446999235, 0.9211410835446999235, 0.9211410835446999235, 0.9211410835446999235, 0.9211410835446999235, 0.9211410835446999235, 0.9211410835446999235),
 ( 1.236576749365999817, 1.236576749365999817, 1.236576749365999817, 1.236576749365999817, 1.236576749365999817, 1.236576749365999817, 1.236576749365999817, 1.236576749365999817, 1.236576749365999817, 1.236576749365999817, 1.236576749365999817, 1.236576749365999817, 1.236576749365999817, 1.236576749365999817, 1.236576749365999817, 1.236576749365999817, 1.236576749365999817, 1.236576749365999817, 1.236576749365999817, 1.236576749365999817, 1.236576749365999817, 1.236576749365999817, 1.236576749365999817, 1.236576749365999817, 1.236576749365999817, 1.236576749365999817, 1.236576749365999817, 1.236576749365999817, 1.236576749365999817, 1.236576749365999817, 1.236576749365999817, 1.236576749365999817, 1.236576749365999817, 1.236576749365999817, 1.236576749365999817, 1.236576749365999817, 1.236576749365999817, 1.236576749365999817, 1.236576749365999817, 1.236576749365999817, 1.236576749365999817, 1.236576749365999817, 1.236576749365999817, 1.236576749365999817, 1.236576749365999817, 1.236576749365999817, 1.236576749365999817, 1.236576749365999817, 1.236576749365999817, 1.236576749365999817) ) ) 
 REPRESENTATION_ITEM ( '' )  SURFACE ( )  );
#3672 = AXIS2_PLACEMENT_3D ( 'NONE', #6674, #9953, #2594 ) ;
#3673 = CARTESIAN_POINT ( 'NONE',  ( 17.50000000000000000, 0.000000000000000000, -315.0000000000000000 ) ) ;
#3674 = ORIENTED_EDGE ( 'NONE', *, *, #6824, .F. ) ;
#3675 = AXIS2_PLACEMENT_3D ( 'NONE', #1134, #7690, #10109 ) ;
#3676 = CARTESIAN_POINT ( 'NONE',  ( 14.90286285339066019, 5.148601615201705783, -314.5782021036098968 ) ) ;
#3677 = CIRCLE ( 'NONE', #1795, 15.00000000000002487 ) ;
#3679 = ORIENTED_EDGE ( 'NONE', *, *, #8962, .T. ) ;
#3678 = VECTOR ( 'NONE', #783, 1000.000000000000000 ) ;
#3680 =( LENGTH_UNIT ( ) NAMED_UNIT ( * ) SI_UNIT ( .MILLI., .METRE. ) );
#3681 = DIRECTION ( 'NONE',  ( -0.8820010751365675583, 0.000000000000000000, -0.4712473909295825103 ) ) ;
#3682 = ORIENTED_EDGE ( 'NONE', *, *, #3149, .T. ) ;
#3683 = LINE ( 'NONE', #2123, #2439 ) ;
#3684 = ORIENTED_EDGE ( 'NONE', *, *, #444, .F. ) ;
#3685 = DIRECTION ( 'NONE',  ( -0.000000000000000000, 1.000000000000000000, 0.000000000000000000 ) ) ;
#3686 = CARTESIAN_POINT ( 'NONE',  ( -0.1580967862520001599, -11.39739484195000330, -302.5071922382879279 ) ) ;
#3687 = CYLINDRICAL_SURFACE ( 'NONE', #4890, 14.99999999999999467 ) ;
#3688 = ORIENTED_EDGE ( 'NONE', *, *, #821, .F. ) ;
#3689 = AXIS2_PLACEMENT_3D ( 'NONE', #9599, #3959, #7239 ) ;
#3690 = FACE_OUTER_BOUND ( 'NONE', #7450, .T. ) ;
#3691 = CARTESIAN_POINT ( 'NONE',  ( 18.27982664221999443, 2.925785484622998922, -302.5071922382879279 ) ) ;
#3692 = CARTESIAN_POINT ( 'NONE',  ( -13.19336277821000536, -9.492603533888004819, 319.5792614743400009 ) ) ;
#3693 = CARTESIAN_POINT ( 'NONE',  ( 17.59298685096999648, -0.02218567204016000036, -314.4150829855000211 ) ) ;
#3694 = CARTESIAN_POINT ( 'NONE',  ( 1.285290206351000108, 10.09749793447999977, 314.4150829855000211 ) ) ;
#3695 = ORIENTED_EDGE ( 'NONE', *, *, #4169, .T. ) ;
#3696 = CARTESIAN_POINT ( 'NONE',  ( -19.96251415050936728, -0.9422375983257673671, 190.9999999999995737 ) ) ;
#3697 = ORIENTED_EDGE ( 'NONE', *, *, #3049, .F. ) ;
#3698 = CARTESIAN_POINT ( 'NONE',  ( -0.7938766977148212778, -7.490427039502949746, -434.2959395039480341 ) ) ;
#3699 = FACE_BOUND ( 'NONE', #6668, .T. ) ;
#3700 = EDGE_CURVE ( 'NONE', #189, #1010, #900, .T. ) ;
#3701 = CARTESIAN_POINT ( 'NONE',  ( -17.14610219660000112, -0.04370646908743999748, 314.8616023057000461 ) ) ;
#3702 = CARTESIAN_POINT ( 'NONE',  ( -16.35728328174216273, 2.567538628164302228, 315.0000000000000568 ) ) ;
#3703 = FACE_BOUND ( 'NONE', #94, .T. ) ;
#3704 = PRODUCT_DEFINITION_FORMATION_WITH_SPECIFIED_SOURCE ( 'ANY', '', #1232, .NOT_KNOWN. ) ;
#3705 = CARTESIAN_POINT ( 'NONE',  ( -16.33391464646021518, -2.612996577909529883, -315.0000000000000000 ) ) ;
#3706 = CARTESIAN_POINT ( 'NONE',  ( -20.00000000024866864, 25.00000000007771561, 191.0000000000000000 ) ) ;
#3707 = EDGE_CURVE ( 'NONE', #6146, #4332, #5195, .T. ) ;
#3708 = DIRECTION ( 'NONE',  ( -0.9942380540931650135, 0.000000000000000000, -0.1071946444232960011 ) ) ;
#3709 = CARTESIAN_POINT ( 'NONE',  ( 20.00000000000000000, 0.000000000000000000, -316.5000000000000000 ) ) ;
#3710 = EDGE_CURVE ( 'NONE', #7593, #471, #154, .T. ) ;
#3711 = B_SPLINE_CURVE_WITH_KNOTS ( 'NONE', 3,
 ( #3557, #3655, #6073, #4310, #9363, #5262, #8537, #9951, #5054, #1944, #7581, #5212, #1892, #6787, #9145, #973, #1179, #4460, #10059, #2700, #5163, #8435, #1075, #4363, #278, #10219, #3756, #9410, #1606, #3813, #2407, #5675, #1288, #10266, #10367, #7100, #6941, #2903, #5313, #8586, #3712, #3873, #6994, #7150, #1393, #8749, #6172, #2854, #7788, #6226, #6122, #4676, #596, #7951, #2953, #8642, #9458, #1231, #2097, #7841, #2045, #3008, #6283, #9769, #9512, #488, #9562, #2203, #2152, #1339, #5473, #4567, #8960, #10418, #3060, #5362, #6491, #4878, #5417, #7047, #8156, #794, #539, #4509, #433, #10315, #8693, #4619, #7892, #8415, #9821, #8308, #9878, #949, #3374, #843, #1867, #6543, #4288, #4233, #4127, #2622, #3481, #205, #5728, #1653, #2461, #7352, #894, #9018, #9235, #7507, #10034, #2678, #9071, #7403, #149, #3423, #4073, #42, #4929, #1706, #5884, #4979, #8206, #2515 ),
 .UNSPECIFIED., .F., .F.,
 ( 4, 1, 1, 1, 1, 1, 2, 2, 1, 1, 1, 1, 1, 2, 2, 1, 1, 1, 1, 1, 2, 2, 1, 1, 1, 1, 1, 2, 2, 1, 1, 1, 1, 1, 1, 2, 2, 1, 1, 1, 1, 1, 2, 2, 1, 1, 2, 2, 2, 1, 1, 2, 2, 1, 1, 1, 1, 2, 2, 1, 1, 1, 1, 1, 1, 2, 2, 1, 1, 1, 1, 1, 2, 2, 1, 1, 1, 1, 1, 2, 2, 1, 1, 1, 1, 1, 2, 2, 1, 1, 1, 1, 2, 2, 4 ),
 ( 0.000000000000000000, 0.06250000000000710543, 0.09375000000001064426, 0.1093750000000124206, 0.1171875000000132394, 0.1210937500000135447, 0.1230468750000136002, 0.1250000000000136557, 0.1562500000000150158, 0.1718750000000157097, 0.1796875000000160705, 0.1835937500000162925, 0.1855468750000164035, 0.1865234375000164868, 0.1875000000000165701, 0.2187500000000191513, 0.2343750000000204836, 0.2421875000000211775, 0.2460937500000215383, 0.2480468750000217881, 0.2490234375000218991, 0.2500000000000219824, 0.2812500000000247580, 0.2968750000000262013, 0.3046875000000269784, 0.3085937500000273115, 0.3105468750000274225, 0.3115234375000274225, 0.3125000000000274225, 0.3437500000000277556, 0.3593750000000279776, 0.3671875000000280886, 0.3710937500000281442, 0.3730468750000281997, 0.3740234375000283107, 0.3745117187500283107, 0.3750000000000283107, 0.4062500000000291434, 0.4218750000000295319, 0.4296875000000297540, 0.4335937500000298650, 0.4355468750000299205, 0.4365234375000299205, 0.4375000000000299205, 0.4531250000000300315, 0.4609375000000300870, 0.4648437500000301426, 0.4687500000000301981, 0.5000000000000304201, 0.5156250000000306422, 0.5234375000000307532, 0.5273437500000307532, 0.5312500000000307532, 0.5468750000000309752, 0.5546875000000310862, 0.5585937500000310862, 0.5605468750000310862, 0.5615234375000310862, 0.5625000000000310862, 0.5937500000000295319, 0.6093750000000287548, 0.6171875000000284217, 0.6210937500000283107, 0.6230468750000281997, 0.6240234375000281997, 0.6245117187500281997, 0.6250000000000283107, 0.6562500000000291989, 0.6718750000000295319, 0.6796875000000297540, 0.6835937500000298650, 0.6855468750000299760, 0.6865234375000299760, 0.6875000000000299760, 0.7187500000000308642, 0.7343750000000313083, 0.7421875000000315303, 0.7460937500000316414, 0.7480468750000317524, 0.7490234375000317524, 0.7500000000000317524, 0.7812500000000317524, 0.7968750000000316414, 0.8046875000000316414, 0.8085937500000316414, 0.8105468750000315303, 0.8115234375000314193, 0.8125000000000313083, 0.8437500000000284217, 0.8593750000000270894, 0.8671875000000264233, 0.8710937500000259792, 0.8730468750000257572, 0.8750000000000255351, 1.000000000000000000 ),
 .UNSPECIFIED. ) ;
#3712 = CARTESIAN_POINT ( 'NONE',  ( -9.142617743994909674, 7.997268146336696581, -315.0000000000000568 ) ) ;
#3713 = CARTESIAN_POINT ( 'NONE',  ( -7.659536309752155603, -8.000000000000000000, -398.9184288142485570 ) ) ;
#3714 = DIRECTION ( 'NONE',  ( 0.9942380540931650135, 0.000000000000000000, 0.1071946444232960011 ) ) ;
#3715 = CARTESIAN_POINT ( 'NONE',  ( 6.668310453960305750, -4.452685652811780415, -525.2390882416690374 ) ) ;
#3716 = CARTESIAN_POINT ( 'NONE',  ( 0.000000000000000000, 0.000000000000000000, 315.0000000000000000 ) ) ;
#3717 = CARTESIAN_POINT ( 'NONE',  ( 16.13945612244922501, -2.966804785441415238, 314.9999999999999432 ) ) ;
#3718 = CARTESIAN_POINT ( 'NONE',  ( 14.52969073417999901, 5.422537850045999974, -314.6383426456000052 ) ) ;
#3719 = ADVANCED_FACE ( 'NONE', ( #1115 ), #7565, .T. ) ;
#3720 = CARTESIAN_POINT ( 'NONE',  ( 9.801936311039993299, 9.714404437230999889, 319.9928079742500131 ) ) ;
#3721 = CARTESIAN_POINT ( 'NONE',  ( -85.79375217459825365, -2.500000000000000000, -343.3529193039154279 ) ) ;
#3722 = DIRECTION ( 'NONE',  ( -0.2951854283188042882, 0.000000000000000000, 0.9554399839384178916 ) ) ;
#3723 = ORIENTED_EDGE ( 'NONE', *, *, #3440, .T. ) ;
#3724 = CARTESIAN_POINT ( 'NONE',  ( -18.29581373626999508, 2.889895519923001643, -317.4928077629770087 ) ) ;
#3725 = CARTESIAN_POINT ( 'NONE',  ( 18.63147570264002084, -4.749337304460001796, -317.0792622552969533 ) ) ;
#3726 = PRODUCT ( 'Upper Cutting Blade', 'Upper Cutting Blade', '', ( #9676 ) ) ;
#3727 = CARTESIAN_POINT ( 'NONE',  ( -17.50000000000000000, 0.000000000000000000, -315.0000000000000000 ) ) ;
#3728 = CARTESIAN_POINT ( 'NONE',  ( -0.9068124364724808872, 10.00021929074745231, -314.4998859403474398 ) ) ;
#3729 = ORIENTED_EDGE ( 'NONE', *, *, #5744, .F. ) ;
#3730 = CARTESIAN_POINT ( 'NONE',  ( -10.60011422839999895, -9.531420659438001763, 190.0000000000000000 ) ) ;
#3731 = LINE ( 'NONE', #10290, #6781 ) ;
#3732 = ORIENTED_EDGE ( 'NONE', *, *, #1203, .T. ) ;
#3733 = CARTESIAN_POINT ( 'NONE',  ( -14.79481407445002183, -8.414248563823001348, 191.1197171614399792 ) ) ;
#3734 = ORIENTED_EDGE ( 'NONE', *, *, #10029, .T. ) ;
#3735 = CARTESIAN_POINT ( 'NONE',  ( 8.907970405212992659, -10.02857016715000604, -302.5071922382879279 ) ) ;
#3736 = LINE ( 'NONE', #7024, #5911 ) ;
#3737 = AXIS2_PLACEMENT_3D ( 'NONE', #752, #2, #805 ) ;
#3738 = CARTESIAN_POINT ( 'NONE',  ( -0.7261718205266309845, -7.501926320342999333, -434.1735064888349029 ) ) ;
#3739 = CARTESIAN_POINT ( 'NONE',  ( -1.615578127792000274, 11.35484692374000737, -302.5071922382879279 ) ) ;
#3740 = CARTESIAN_POINT ( 'NONE',  ( -17.64852322130001738, -5.886271888320000478, 318.8802828394900644 ) ) ;
#3741 = CARTESIAN_POINT ( 'NONE',  ( -45.40077937890500692, -9.500000000000001776, -426.7517346751886862 ) ) ;
#3742 = CARTESIAN_POINT ( 'NONE',  ( -16.41165915566000066, 2.800979832323999830, 314.8616023057000461 ) ) ;
#3743 = EDGE_LOOP ( 'NONE', ( #3841, #3110, #8398, #3152 ) ) ;
#3744 = CARTESIAN_POINT ( 'NONE',  ( 9.745026809365992193, -9.735374599634990744, 190.0071920248299477 ) ) ;
#3745 = ORIENTED_EDGE ( 'NONE', *, *, #1436, .T. ) ;
#3746 = CARTESIAN_POINT ( 'NONE',  ( 11.22625503481000209, 10.34655023142000907, 318.8802828394900644 ) ) ;
#3747 = DIRECTION ( 'NONE',  ( -1.000000000000000000, 0.000000000000000000, 0.000000000000000000 ) ) ;
#3748 = CARTESIAN_POINT ( 'NONE',  ( -76.33371517498638070, -7.500000000000000000, -329.2281998388791635 ) ) ;
#3749 = CARTESIAN_POINT ( 'NONE',  ( -10.00000000000000000, -2.500000000000000000, -317.5000000000000000 ) ) ;
#3750 = CARTESIAN_POINT ( 'NONE',  ( -16.74588786138889063, 1.629246332199927538, 315.0000000000000000 ) ) ;
#3751 = CARTESIAN_POINT ( 'NONE',  ( -46.74071243419621169, -9.500000000000001776, -414.3237589990241077 ) ) ;
#3752 = CARTESIAN_POINT ( 'NONE',  ( -4.578722611353294170, -9.145541810471781830, -315.0000000000000568 ) ) ;
#3753 = CARTESIAN_POINT ( 'NONE',  ( -20.00000000024866864, 25.00000000007771561, 319.0000000000000000 ) ) ;
#3754 = DIRECTION ( 'NONE',  ( -1.000000000000000000, 0.000000000000000000, 0.000000000000000000 ) ) ;
#3755 = FACE_OUTER_BOUND ( 'NONE', #1188, .T. ) ;
#3756 = CARTESIAN_POINT ( 'NONE',  ( -13.98368610735814421, 5.377133503752142829, -315.0000000000000568 ) ) ;
#3757 = CARTESIAN_POINT ( 'NONE',  ( 11.86325706386000434, 9.609314883874001012, 189.9229057364800042 ) ) ;
#3758 = VERTEX_POINT ( 'NONE', #7461 ) ;
#3759 = CARTESIAN_POINT ( 'NONE',  ( 6.666144892128035515, -4.452904620723932005, -525.2371525738265063 ) ) ;
#3760 = CIRCLE ( 'NONE', #6162, 3.500000000000003109 ) ;
#3761 = AXIS2_PLACEMENT_3D ( 'NONE', #9004, #6690, #881 ) ;
#3762 = CARTESIAN_POINT ( 'NONE',  ( 10.00000000000000000, 2.500000000000000000, -317.5000000000000000 ) ) ;
#3763 = DIRECTION ( 'NONE',  ( 1.000000000000000000, 0.000000000000000000, 0.000000000000000000 ) ) ;
#3764 = CARTESIAN_POINT ( 'NONE',  ( 16.83787941357387297, -1.297844089352232944, 315.0000000000000568 ) ) ;
#3765 = CARTESIAN_POINT ( 'NONE',  ( -8.690073206612000334, 8.569658446474999636, -314.6383426456000052 ) ) ;
#3766 = LINE ( 'NONE', #5483, #7208 ) ;
#3767 = CARTESIAN_POINT ( 'NONE',  ( 17.33400069613001193, 5.617198899843996784, 320.0770942683900557 ) ) ;
#3768 = DIRECTION ( 'NONE',  ( 0.000000000000000000, 1.000000000000000000, -0.000000000000000000 ) ) ;
#3769 = CARTESIAN_POINT ( 'NONE',  ( -1.685183431873553461, -2.689364145315999099, -435.0748299022583296 ) ) ;
#3770 = ORIENTED_EDGE ( 'NONE', *, *, #10207, .T. ) ;
#3771 = CARTESIAN_POINT ( 'NONE',  ( -17.80394872498997927, 5.851108818846995518, -317.0792622552969533 ) ) ;
#3772 = VECTOR ( 'NONE', #8162, 1000.000000000000000 ) ;
#3773 = CARTESIAN_POINT ( 'NONE',  ( -17.39473599676002635, -5.562790558317003864, -317.5770954168139610 ) ) ;
#3774 = EDGE_CURVE ( 'NONE', #3885, #9012, #7934, .T. ) ;
#3775 =( BOUNDED_CURVE ( )  B_SPLINE_CURVE ( 3, ( #4208, #7482, #6625, #3346 ),
 .UNSPECIFIED., .F., .T. ) 
 B_SPLINE_CURVE_WITH_KNOTS ( ( 4, 4 ),
 ( 1.013329913875473588E-09, 1.000000000000000000 ),
 .UNSPECIFIED. ) 
 CURVE ( )  GEOMETRIC_REPRESENTATION_ITEM ( )  RATIONAL_B_SPLINE_CURVE ( ( 0.9922218186767667314, 0.8003084390180068564, 0.8029011661257512422, 1.000000000000000000 ) ) 
 REPRESENTATION_ITEM ( '' )  );
#3776 = CARTESIAN_POINT ( 'NONE',  ( -12.98706127646999953, -6.788989183774999603, -315.0000000000000000 ) ) ;
#3777 = EDGE_CURVE ( 'NONE', #4923, #168, #8279, .T. ) ;
#3778 = ADVANCED_BREP_SHAPE_REPRESENTATION ( '', ( #1695, #2817 ), #7476 ) ;
#3779 = CIRCLE ( 'NONE', #2244, 0.5000000000000004441 ) ;
#3780 = LINE ( 'NONE', #10126, #49 ) ;
#3781 = ORIENTED_EDGE ( 'NONE', *, *, #6819, .F. ) ;
#3782 = AXIS2_PLACEMENT_3D ( 'NONE', #1675, #861, #813 ) ;
#3783 = CARTESIAN_POINT ( 'NONE',  ( -11.72056399716000108, 9.035224326960999974, 190.0000000000000000 ) ) ;
#3784 = CARTESIAN_POINT ( 'NONE',  ( 0.6338995735901449269, -12.51432109910909851, 319.0000000000003979 ) ) ;
#3785 = ORIENTED_EDGE ( 'NONE', *, *, #4128, .T. ) ;
#3786 = CARTESIAN_POINT ( 'NONE',  ( 15.61478958302000208, -7.813810907915007320, 191.1197171614399792 ) ) ;
#3787 = ORIENTED_EDGE ( 'NONE', *, *, #4113, .T. ) ;
#3788 = CARTESIAN_POINT ( 'NONE',  ( -1.514431797236434930E-09, -10.00000000000000000, -302.5000000000000000 ) ) ;
#3789 = CARTESIAN_POINT ( 'NONE',  ( 13.72185241754999652, -8.618935511841003816, -302.4229045757450081 ) ) ;
#3790 = EDGE_CURVE ( 'NONE', #2499, #111, #9477, .T. ) ;
#3791 = CARTESIAN_POINT ( 'NONE',  ( 11.02833964697000013, 10.42949886550000826, 191.1197171614399792 ) ) ;
#3792 = VERTEX_POINT ( 'NONE', #48 ) ;
#3793 = CARTESIAN_POINT ( 'NONE',  ( -1.367705781936138676, -7.477163225200000873, -434.5183335501718602 ) ) ;
#3794 = CARTESIAN_POINT ( 'NONE',  ( 19.56012101500002132, -0.5268190066377996805, -302.4229045757450081 ) ) ;
#3795 = APPLICATION_CONTEXT ( 'automotive_design' ) ;
#3796 = CARTESIAN_POINT ( 'NONE',  ( 17.50000000000000000, 0.000000000000000000, -315.0000000000000000 ) ) ;
#3797 = CARTESIAN_POINT ( 'NONE',  ( -6.419414596134000561, -9.427679607337001499, -314.4150829855000211 ) ) ;
#3798 = CARTESIAN_POINT ( 'NONE',  ( -17.59298685096999648, 0.02218567204014999794, 314.4150829855000211 ) ) ;
#3799 = ORIENTED_EDGE ( 'NONE', *, *, #6141, .T. ) ;
#3800 = CARTESIAN_POINT ( 'NONE',  ( 18.89081873304001036, -0.08752760549137006407, 190.0071920248299477 ) ) ;
#3801 = CARTESIAN_POINT ( 'NONE',  ( -6.038923639677001631, 11.92375595181999870, 318.8802828394900644 ) ) ;
#3802 = CARTESIAN_POINT ( 'NONE',  ( -82.96626782902075092, -2.366295999999999733, -348.6449257547347997 ) ) ;
#3803 = ADVANCED_FACE ( 'NONE', ( #5891 ), #9932, .F. ) ;
#3804 = VERTEX_POINT ( 'NONE', #9187 ) ;
#3805 = DIRECTION ( 'NONE',  ( 0.000000000000000000, -1.000000000000000000, 0.000000000000000000 ) ) ;
#3806 = PLANE ( 'NONE',  #6070 ) ;
#3807 = FACE_OUTER_BOUND ( 'NONE', #10083, .T. ) ;
#3808 = CARTESIAN_POINT ( 'NONE',  ( -17.50000000000000000, 1.896400240175167841E-08, 314.4999014931028682 ) ) ;
#3809 = CARTESIAN_POINT ( 'NONE',  ( -13.95711901494857088, -5.398584340276485705, -315.0000000000000000 ) ) ;
#3810 = CARTESIAN_POINT ( 'NONE',  ( -3.925578656483873274, -2.997421157293520544, -436.2071454890248674 ) ) ;
#3811 = SURFACE_STYLE_FILL_AREA ( #3006 ) ;
#3812 = CARTESIAN_POINT ( 'NONE',  ( -1.399732096967147621, -7.968300772759999262, -436.0948124694132844 ) ) ;
#3813 = CARTESIAN_POINT ( 'NONE',  ( -13.12058949809353514, 6.031889286829743568, -315.0000000000000568 ) ) ;
#3814 = PRODUCT_DEFINITION_SHAPE ( 'NONE', 'NONE',  #10625 ) ;
#3815 = CARTESIAN_POINT ( 'NONE',  ( -19.57080534385999471, -0.3817780055853002841, 189.9229057364800042 ) ) ;
#3816 = CARTESIAN_POINT ( 'NONE',  ( 6.176342442900598861, 9.366307578403514356, 314.4999456809352978 ) ) ;
#3817 = AXIS2_PLACEMENT_3D ( 'NONE', #1822, #10041, #6602 ) ;
#3818 = ADVANCED_FACE ( 'NONE', ( #2570 ), #5143, .T. ) ;
#3819 = CARTESIAN_POINT ( 'NONE',  ( 7.807700195763000117, -10.48319479899000051, -317.5000000000000000 ) ) ;
#3820 = DIRECTION ( 'NONE',  ( 0.000000000000000000, -1.000000000000000000, 0.000000000000000000 ) ) ;
#3821 = CARTESIAN_POINT ( 'NONE',  ( 15.06605725946605112, -4.378913172242680396, 314.9999999999999432 ) ) ;
#3822 = CARTESIAN_POINT ( 'NONE',  ( -1.409290114754000012, 9.868237606049000021, -314.6383426456000052 ) ) ;
#3823 = CARTESIAN_POINT ( 'NONE',  ( -16.98100918689000238, -2.500000000000000000, -439.4179428962999623 ) ) ;
#3824 = AXIS2_PLACEMENT_3D ( 'NONE', #4641, #9584, #617 ) ;
#3825 = CARTESIAN_POINT ( 'NONE',  ( -7.392698694382005442, 11.19283382348000622, 320.0770942683900557 ) ) ;
#3826 = DIRECTION ( 'NONE',  ( -0.3420201433256988555, 0.000000000000000000, 0.9396926207858975477 ) ) ;
#3827 = DIRECTION ( 'NONE',  ( 0.000000000000000000, -1.000000000000000000, 0.000000000000000000 ) ) ;
#3828 = VERTEX_POINT ( 'NONE', #9883 ) ;
#3829 = CARTESIAN_POINT ( 'NONE',  ( -19.95938911887002831, 1.720557998077001827, -317.0792622552969533 ) ) ;
#3830 = FACE_OUTER_BOUND ( 'NONE', #7171, .T. ) ;
#3831 = EDGE_CURVE ( 'NONE', #9889, #2499, #5838, .T. ) ;
#3832 = DIRECTION ( 'NONE',  ( 0.000000000000000000, 1.000000000000000000, 0.000000000000000000 ) ) ;
#3833 = CARTESIAN_POINT ( 'NONE',  ( 14.00000000000000000, 2.500000000000000000, -317.5000000000000000 ) ) ;
#3834 = VERTEX_POINT ( 'NONE', #2684 ) ;
#3835 = CARTESIAN_POINT ( 'NONE',  ( -7.592156631695000435, 10.54118908926000131, 190.0000000000000000 ) ) ;
#3836 = EDGE_CURVE ( 'NONE', #8773, #4852, #1764, .T. ) ;
#3837 = CARTESIAN_POINT ( 'NONE',  ( -17.50000000158811986, -0.4607171203178571650, -314.4995147730188023 ) ) ;
#3838 =( GEOMETRIC_REPRESENTATION_CONTEXT ( 3 ) GLOBAL_UNCERTAINTY_ASSIGNED_CONTEXT ( ( #1844 ) ) GLOBAL_UNIT_ASSIGNED_CONTEXT ( ( #3000, #6380, #9608 ) ) REPRESENTATION_CONTEXT ( 'NONE', 'WORKASPACE' ) );
#3839 = ORIENTED_EDGE ( 'NONE', *, *, #2317, .T. ) ;
#3840 = DIRECTION ( 'NONE',  ( 0.000000000000000000, 0.000000000000000000, 1.000000000000000000 ) ) ;
#3841 = ORIENTED_EDGE ( 'NONE', *, *, #641, .F. ) ;
#3842 = CARTESIAN_POINT ( 'NONE',  ( -9.619189022994751426, -7.822639675800805215, 315.0000000000000000 ) ) ;
#3843 = CARTESIAN_POINT ( 'NONE',  ( 17.42451203059000520, -5.527343733032997974, -302.4229045757450081 ) ) ;
#3844 = EDGE_CURVE ( 'NONE', #10456, #8766, #2079, .T. ) ;
#3845 = AXIS2_PLACEMENT_3D ( 'NONE', #10501, #8780, #8195 ) ;
#3846 = CARTESIAN_POINT ( 'NONE',  ( 19.50564046359999537, 2.789525877152000621, 191.1197171614399792 ) ) ;
#3847 = ORIENTED_EDGE ( 'NONE', *, *, #9891, .T. ) ;
#3848 = VECTOR ( 'NONE', #3875, 1000.000000000000000 ) ;
#3849 =( GEOMETRIC_REPRESENTATION_CONTEXT ( 3 ) GLOBAL_UNCERTAINTY_ASSIGNED_CONTEXT ( ( #7536 ) ) GLOBAL_UNIT_ASSIGNED_CONTEXT ( ( #4615, #430, #10154 ) ) REPRESENTATION_CONTEXT ( 'NONE', 'WORKASPACE' ) );
#3850 = CLOSED_SHELL ( 'NONE', ( #2883, #9333, #8529, #8597, #3260 ) ) ;
#3851 = CARTESIAN_POINT ( 'NONE',  ( -7.818484572095996121, 11.08186606788998674, -302.4229045757450081 ) ) ;
#3852 = CARTESIAN_POINT ( 'NONE',  ( 19.97284803234999018, 0.5555888903174002191, 318.8802828394900644 ) ) ;
#3853 = VERTEX_POINT ( 'NONE', #8620 ) ;
#3854 = CARTESIAN_POINT ( 'NONE',  ( -14.23799507159000122, -5.083276007328000112, -315.0848619657999734 ) ) ;
#3855 = ADVANCED_FACE ( 'NONE', ( #10195 ), #1414, .T. ) ;
#3856 = CARTESIAN_POINT ( 'NONE',  ( 17.62021515802999971, 4.315182425209999728, -302.4999999999969873 ) ) ;
#3857 = ORIENTED_EDGE ( 'NONE', *, *, #5482, .F. ) ;
#3858 = CARTESIAN_POINT ( 'NONE',  ( -7.457264729102998757, -11.17642278912000720, 189.9229057364800042 ) ) ;
#3859 = CARTESIAN_POINT ( 'NONE',  ( -18.68148959551998445, 4.475099553145003739, 318.8802828394900644 ) ) ;
#3860 = DIRECTION ( 'NONE',  ( 0.000000000000000000, -1.000000000000000000, 0.000000000000000000 ) ) ;
#3861 = TOROIDAL_SURFACE ( 'NONE', #262, 12.00000000000000000, 0.5000000000000000000 ) ;
#3862 = AXIS2_PLACEMENT_3D ( 'NONE', #6477, #9758, #5663 ) ;
#3863 = ORIENTED_EDGE ( 'NONE', *, *, #6141, .F. ) ;
#3864 = CARTESIAN_POINT ( 'NONE',  ( -16.58659719219999928, -2.947707964209000053, 314.6383426456000052 ) ) ;
#3865 = CARTESIAN_POINT ( 'NONE',  ( 10.19111474148932395, -9.999999291614226848, 315.0000000000000000 ) ) ;
#3866 = CARTESIAN_POINT ( 'NONE',  ( -15.26162423979700300, 4.160529437000930031, 314.9999999999999432 ) ) ;
#3867 = CARTESIAN_POINT ( 'NONE',  ( -10.79243608611000305, -9.321647281761997306, 319.9928079742500131 ) ) ;
#3868 = CARTESIAN_POINT ( 'NONE',  ( -13.37774034208871754, -5.841704189632142885, -315.0000000000001137 ) ) ;
#3869 = CARTESIAN_POINT ( 'NONE',  ( -14.93448127581804385, -4.114638024020168316, -438.6307627169820194 ) ) ;
#3870 = DIRECTION ( 'NONE',  ( -0.2756373558170050475, 0.000000000000000000, 0.9612616959383172288 ) ) ;
#3871 = VERTEX_POINT ( 'NONE', #6264 ) ;
#3872 = CARTESIAN_POINT ( 'NONE',  ( -0.5534908175310586653, -2.500000333914000006, -434.2941325283891274 ) ) ;
#3873 = CARTESIAN_POINT ( 'NONE',  ( -8.900723324022980165, 8.081813809772741664, -315.0000000000000000 ) ) ;
#3874 = CARTESIAN_POINT ( 'NONE',  ( -19.56918397773000962, 2.861069655901001152, 190.4207385301700128 ) ) ;
#3875 = DIRECTION ( 'NONE',  ( 0.000000000000000000, -1.000000000000000000, 0.000000000000000000 ) ) ;
#3876 = CARTESIAN_POINT ( 'NONE',  ( -20.00000000000000000, 7.277416212200430041E-10, -303.5000000000000000 ) ) ;
#3877 = PLANE ( 'NONE',  #10166 ) ;
#3878 = SHAPE_DEFINITION_REPRESENTATION ( #4584, #1806 ) ;
#3879 = DIRECTION ( 'NONE',  ( -0.8820010751365675583, 0.000000000000000000, -0.4712473909295827323 ) ) ;
#3880 = FACE_OUTER_BOUND ( 'NONE', #4914, .T. ) ;
#3881 = CYLINDRICAL_SURFACE ( 'NONE', #3439, 4.000000000000000000 ) ;
#3882 = CARTESIAN_POINT ( 'NONE',  ( -15.57034186525998543, 6.406527364046002759, 319.9928079742500131 ) ) ;
#3883 = CARTESIAN_POINT ( 'NONE',  ( -46.36553117871467578, -9.500000000000001776, -417.8035921883502510 ) ) ;
#3884 = CARTESIAN_POINT ( 'NONE',  ( -1.793484850425402621, -2.651676682486001191, -434.8900474484831875 ) ) ;
#3885 = VERTEX_POINT ( 'NONE', #1318 ) ;
#3886 = CARTESIAN_POINT ( 'NONE',  ( 15.65816392223999820, 7.257913545763996055, -317.5770954168139610 ) ) ;
#3887 = CARTESIAN_POINT ( 'NONE',  ( -19.12867493021229492, 3.682770601350500606, 319.0000000000005116 ) ) ;
#3888 = CARTESIAN_POINT ( 'NONE',  ( -4.976995723842001951, -12.11314212604000318, -316.3802825947000201 ) ) ;
#3889 = DIRECTION ( 'NONE',  ( 0.000000000000000000, 1.000000000000000000, -0.000000000000000000 ) ) ;
#3890 = CARTESIAN_POINT ( 'NONE',  ( -17.48550435259291191, 0.4594173590775618710, -314.5005290240522413 ) ) ;
#3891 = ORIENTED_EDGE ( 'NONE', *, *, #7244, .F. ) ;
#3892 = CARTESIAN_POINT ( 'NONE',  ( -16.94482484090575269, -2.428629253473818306, -314.5323066871360993 ) ) ;
#3893 = EDGE_CURVE ( 'NONE', #1689, #7605, #1979, .T. ) ;
#3894 = ORIENTED_EDGE ( 'NONE', *, *, #1995, .T. ) ;
#3895 = CARTESIAN_POINT ( 'NONE',  ( -15.96117728870900088, 7.554047240424474730, -316.5000000000004547 ) ) ;
#3896 = VERTEX_POINT ( 'NONE', #6923 ) ;
#3897 = CARTESIAN_POINT ( 'NONE',  ( -8.691248314156576171, -8.152891913651146183, 315.0000000000001137 ) ) ;
#3898 = CARTESIAN_POINT ( 'NONE',  ( -11.73636226353998779, -10.21860227534999943, -302.9207377450070453 ) ) ;
#3899 = DIRECTION ( 'NONE',  ( 0.000000000000000000, -1.000000000000000000, 0.000000000000000000 ) ) ;
#3900 = ADVANCED_FACE ( 'NONE', ( #364 ), #7639, .T. ) ;
#3901 = CARTESIAN_POINT ( 'NONE',  ( -4.978480136836995307, 11.69377972944999478, -302.4229045757450081 ) ) ;
#3902 = PRODUCT_DEFINITION_SHAPE ( 'NONE', 'NONE',  #10624 ) ;
#3903 = CARTESIAN_POINT ( 'NONE',  ( -1.327417525529001496, -12.48520226272998990, 318.8802828394900644 ) ) ;
#3904 = ORIENTED_EDGE ( 'NONE', *, *, #10269, .F. ) ;
#3905 = CARTESIAN_POINT ( 'NONE',  ( 4.061138133959000029, -9.851562218542998295, -314.4150829855000211 ) ) ;
#3906 = CARTESIAN_POINT ( 'NONE',  ( -65.06086774555899410, -8.000000000000000000, -381.4479802600495759 ) ) ;
#3907 = ORIENTED_EDGE ( 'NONE', *, *, #7170, .F. ) ;
#3908 = CARTESIAN_POINT ( 'NONE',  ( 11.00905209676000140, -9.989194338198000622, 189.9229057364800042 ) ) ;
#3909 = VECTOR ( 'NONE', #5305, 1000.000000000000000 ) ;
#3910 = CARTESIAN_POINT ( 'NONE',  ( 13.01454326516111237, 9.502166178128931051, 190.9999999999996589 ) ) ;
#3911 = CARTESIAN_POINT ( 'NONE',  ( -2.000000000000000000, 2.500000000000000000, -409.5000000000000000 ) ) ;
#3912 = EDGE_CURVE ( 'NONE', #574, #9045, #2345, .T. ) ;
#3913 = ORIENTED_EDGE ( 'NONE', *, *, #5468, .T. ) ;
#3914 = ORIENTED_EDGE ( 'NONE', *, *, #36, .T. ) ;
#3915 = CARTESIAN_POINT ( 'NONE',  ( -10.50000150490000017, -7.882579085736000302, 314.6383426456000052 ) ) ;
#3916 = DIRECTION ( 'NONE',  ( -0.8820010751365675583, 0.000000000000000000, -0.4712473909295827323 ) ) ;
#3917 = VECTOR ( 'NONE', #1278, 1000.000000000000227 ) ;
#3918 = CARTESIAN_POINT ( 'NONE',  ( -14.93129073739000034, 7.087303338045999546, 320.0000000000000000 ) ) ;
#3919 = CARTESIAN_POINT ( 'NONE',  ( 2.482300462934001306, -11.29873291818999803, 319.9928079742500131 ) ) ;
#3920 = DIRECTION ( 'NONE',  ( -0.6156614753245235327, 0.000000000000000000, 0.7880107536076085273 ) ) ;
#3921 = CARTESIAN_POINT ( 'NONE',  ( -14.95096017393944976, -4.021413106997576037, -438.5635601240937262 ) ) ;
#3922 = DIRECTION ( 'NONE',  ( -0.1071946444232959872, 0.000000000000000000, 0.9942380540931649024 ) ) ;
#3923 = ORIENTED_EDGE ( 'NONE', *, *, #4838, .T. ) ;
#3924 = DIRECTION ( 'NONE',  ( 0.000000000000000000, -1.000000000000000000, 0.000000000000000000 ) ) ;
#3925 = CARTESIAN_POINT ( 'NONE',  ( 0.7033324871771002851, 12.09174782753000166, 189.9229057364800042 ) ) ;
#3926 = FACE_OUTER_BOUND ( 'NONE', #2381, .T. ) ;
#3927 = EDGE_CURVE ( 'NONE', #1373, #2124, #1911, .T. ) ;
#3928 = FACE_BOUND ( 'NONE', #826, .T. ) ;
#3929 = CARTESIAN_POINT ( 'NONE',  ( 16.04008061823806131, 3.141427272462999021, 315.0000000000000000 ) ) ;
#3930 = APPLICATION_PROTOCOL_DEFINITION ( 'draft international standard', 'automotive_design', 1998, #14 ) ;
#3931 = CARTESIAN_POINT ( 'NONE',  ( 10.00000000000000000, -2.500000000000000000, -272.5000000000000000 ) ) ;
#3932 = CARTESIAN_POINT ( 'NONE',  ( -37.62994892356022092, -9.000000000000001776, -402.7806230189644339 ) ) ;
#3933 = DIRECTION ( 'NONE',  ( -0.9942380540931649024, 0.000000000000000000, -0.1071946444232959872 ) ) ;
#3934 = CARTESIAN_POINT ( 'NONE',  ( 19.11656497511998154, 2.646905232783001605, 320.0770942683900557 ) ) ;
#3935 = DIRECTION ( 'NONE',  ( 0.000000000000000000, -1.000000000000000000, 0.000000000000000000 ) ) ;
#3936 = CARTESIAN_POINT ( 'NONE',  ( -0.9394808717797451525, -2.588107745667998838, -434.7776290900898175 ) ) ;
#3937 = ORIENTED_EDGE ( 'NONE', *, *, #5938, .F. ) ;
#3938 = CARTESIAN_POINT ( 'NONE',  ( -5.336288444022999400, 12.13785676344998699, -317.0792622552969533 ) ) ;
#3939 = CARTESIAN_POINT ( 'NONE',  ( 2.055393166047998932, -12.44351316864999824, -316.3802825947000201 ) ) ;
#3940 = AXIS2_PLACEMENT_3D ( 'NONE', #795, #2565, #9125 ) ;
#3941 = EDGE_CURVE ( 'NONE', #7016, #9158, #3647, .T. ) ;
#3942 = FACE_OUTER_BOUND ( 'NONE', #143, .T. ) ;
#3943 = CARTESIAN_POINT ( 'NONE',  ( -0.6600669447125852018, -9.500000000000001776, -421.9279756761403632 ) ) ;
#3944 = CARTESIAN_POINT ( 'NONE',  ( -9.542482902900836450, -7.500000000000000000, -498.6999609700373526 ) ) ;
#3945 = ORIENTED_EDGE ( 'NONE', *, *, #6205, .F. ) ;
#3946 = CIRCLE ( 'NONE', #7551, 11.99999999999998401 ) ;
#3947 = CARTESIAN_POINT ( 'NONE',  ( -9.075831286667817466, -11.14872141952138485, 319.0000000000003979 ) ) ;
#3948 = ORIENTED_EDGE ( 'NONE', *, *, #8403, .F. ) ;
#3949 = FACE_OUTER_BOUND ( 'NONE', #5599, .T. ) ;
#3950 = ORIENTED_EDGE ( 'NONE', *, *, #10074, .T. ) ;
#3951 = CARTESIAN_POINT ( 'NONE',  ( -4.713955699089914297, -9.123860163919065513, 315.0000000000000568 ) ) ;
#3952 = CARTESIAN_POINT ( 'NONE',  ( -18.60584266697000544, -4.788593885995998889, -302.9207377450070453 ) ) ;
#3953 = CARTESIAN_POINT ( 'NONE',  ( -79.74686404004059170, -2.500000000000000000, -383.9321052860355508 ) ) ;
#3954 = CARTESIAN_POINT ( 'NONE',  ( -75.99363846394659561, -7.500000000000000000, -373.3662649509979587 ) ) ;
#3955 = CARTESIAN_POINT ( 'NONE',  ( -6.550050338814993545, 11.90210887660999184, -302.9207377450070453 ) ) ;
#3956 = CARTESIAN_POINT ( 'NONE',  ( 15.55726960039999973, -7.859060843840002697, 318.8802828394900644 ) ) ;
#3957 = ORIENTED_EDGE ( 'NONE', *, *, #1305, .F. ) ;
#3958 = CARTESIAN_POINT ( 'NONE',  ( 8.551447359560999217, -8.144527334518999240, -315.0848619657999734 ) ) ;
#3959 = DIRECTION ( 'NONE',  ( 0.000000000000000000, -1.000000000000000000, 0.000000000000000000 ) ) ;
#3960 = ORIENTED_EDGE ( 'NONE', *, *, #138, .F. ) ;
#3961 = CARTESIAN_POINT ( 'NONE',  ( -10.87058130030999159, -10.04705985032000370, 189.9229057364800042 ) ) ;
#3962 = CARTESIAN_POINT ( 'NONE',  ( -10.13048420337591615, 10.78707197045944532, 190.9999999999996589 ) ) ;
#3963 = PRODUCT_DEFINITION ( 'UNKNOWN', '', #3023, #6464 ) ;
#3964 = DIRECTION ( 'NONE',  ( 0.000000000000000000, -1.000000000000000000, 0.000000000000000000 ) ) ;
#3965 = CARTESIAN_POINT ( 'NONE',  ( -15.56325459994999960, -4.731967449628999844, 314.4150829855000211 ) ) ;
#3966 = DIRECTION ( 'NONE',  ( 0.000000000000000000, 0.000000000000000000, 1.000000000000000000 ) ) ;
#3967 = CARTESIAN_POINT ( 'NONE',  ( 18.20902923167000154, 3.282017551273999967, 320.0000000000000000 ) ) ;
#3968 = CARTESIAN_POINT ( 'NONE',  ( 12.43797004353999469, -8.540074035031999244, 319.9928079742500131 ) ) ;
#3969 = CARTESIAN_POINT ( 'NONE',  ( 4.928966968695695172, 12.12973353869088200, 319.0000000000005116 ) ) ;
#3970 = CARTESIAN_POINT ( 'NONE',  ( -1.873948611771682149, -12.50000000000000000, -349.2478646809681777 ) ) ;
#3971 = ORIENTED_EDGE ( 'NONE', *, *, #10207, .F. ) ;
#3972 = CARTESIAN_POINT ( 'NONE',  ( 11.28781796570999951, 4.951468039558000633, -285.0000000000000000 ) ) ;
#3973 = EDGE_CURVE ( 'NONE', #5288, #2605, #3780, .T. ) ;
#3974 = CARTESIAN_POINT ( 'NONE',  ( -15.36042613538998758, 7.487426557894995227, 189.9229057364800042 ) ) ;
#3975 = PLANE ( 'NONE',  #2820 ) ;
#3976 = VECTOR ( 'NONE', #5351, 1000.000000000000000 ) ;
#3977 = DIRECTION ( 'NONE',  ( 0.2381566831044827082, 0.000000000000000000, -0.9712267471052632439 ) ) ;
#3978 = CARTESIAN_POINT ( 'NONE',  ( -19.99999035944999903, 7.277427703818000446E-10, -303.5000000000000000 ) ) ;
#3979 = APPLICATION_PROTOCOL_DEFINITION ( 'draft international standard', 'automotive_design', 1998, #1051 ) ;
#3980 = CARTESIAN_POINT ( 'NONE',  ( 8.037373804805000077, 9.179324345868998591, -315.0000000000000000 ) ) ;
#3981 = CARTESIAN_POINT ( 'NONE',  ( 16.39086977655999888, 2.839079766962000040, -314.8616023057000461 ) ) ;
#3982 = EDGE_CURVE ( 'NONE', #9423, #3262, #8509, .T. ) ;
#3983 = DIRECTION ( 'NONE',  ( 0.000000000000000000, 0.000000000000000000, -1.000000000000000000 ) ) ;
#3984 = AXIS2_PLACEMENT_3D ( 'NONE', #6746, #9965, #5867 ) ;
#3985 = EDGE_CURVE ( 'NONE', #4227, #6366, #3576, .T. ) ;
#3986 = CARTESIAN_POINT ( 'NONE',  ( -16.03176714517000079, 6.932210726315004123, 320.0770942683900557 ) ) ;
#3987 = CARTESIAN_POINT ( 'NONE',  ( -1.588630714176977321, -2.677470159135998617, -435.0401446854098708 ) ) ;
#3988 = EDGE_LOOP ( 'NONE', ( #5595, #9385, #1885, #10541 ) ) ;
#3989 = CARTESIAN_POINT ( 'NONE',  ( 18.92046274781997894, 3.214434834450002221, -317.5770954168139610 ) ) ;
#3990 = CARTESIAN_POINT ( 'NONE',  ( 0.2363117521398999110, -12.51008298726001300, -316.3802825947000201 ) ) ;
#3991 = CARTESIAN_POINT ( 'NONE',  ( -7.608551686289999338, -10.53686309807999955, 320.0000000000000000 ) ) ;
#3992 = CARTESIAN_POINT ( 'NONE',  ( -0.9146125851449583566, -7.458905582773998511, -434.9923621525751400 ) ) ;
#3993 = AXIS2_PLACEMENT_3D ( 'NONE', #6988, #6165, #2794 ) ;
#3994 = UNCERTAINTY_MEASURE_WITH_UNIT (LENGTH_MEASURE( 1.000000000000000082E-05 ), #1566, 'distance_accuracy_value', 'NONE');
#3995 = FACE_BOUND ( 'NONE', #1870, .T. ) ;
#3996 = DIRECTION ( 'NONE',  ( -0.1071946444232959872, 0.000000000000000000, 0.9942380540931649024 ) ) ;
#3997 = ORIENTED_EDGE ( 'NONE', *, *, #1423, .T. ) ;
#3998 =( BOUNDED_SURFACE ( )  B_SPLINE_SURFACE ( 3, 3, ( 
 ( #4538, #9338, #7717, #3586, #8464, #5393, #5290, #6972, #7023, #6917, #10189, #6102, #9389, #4393, #2023, #6866, #1055, #7763, #4339, #405, #3686, #2880, #6150, #5995, #2074, #5337, #3735, #8614, #1261, #7816, #462, #10295, #7612, #260, #3535, #6813, #10086, #2727, #1107, #5552, #8840 ),
 ( #3201, #5611, #1422, #8086, #9591, #8779, #6258, #2233, #6473, #7076, #8724, #9755, #1484, #3087, #10344, #10446, #4762, #2179, #10561, #2395, #3145, #1367, #7232, #729, #4815, #2982, #9539, #518, #1315, #5500, #3789, #8673, #4005, #4596, #3843, #7285, #8893, #2287, #7127, #8032, #5446 ),
 ( #4705, #677, #7869, #624, #4650, #3952, #7920, #567, #10394, #7984, #3034, #6307, #3898, #10499, #7177, #1532, #6364, #9645, #6418, #9702, #2342, #3250, #7545, #9914, #934, #988, #9864, #5768, #2502, #6581, #9003, #3300, #4917, #10021, #9056, #6748, #1692, #5816, #4966, #2552, #10608 ),
 ( #8350, #8241, #879, #9111, #1745, #4164, #82, #5014, #7390, #4275, #5869, #8292, #8194, #4219, #7495, #7442, #26, #192, #2608, #3361, #5069, #6638, #136, #6528, #3412, #3466, #4061, #5717, #5661, #6687, #9967, #7337, #9161, #1800, #9809, #8946, #1590, #4866, #1642, #8142, #781 ) ),
 .UNSPECIFIED., .F., .F., .F. ) 
 B_SPLINE_SURFACE_WITH_KNOTS ( ( 4, 4 ),
 ( 4, 1, 1, 1, 1, 1, 1, 1, 1, 1, 1, 1, 1, 1, 1, 1, 1, 1, 1, 1, 1, 1, 1, 1, 1, 1, 1, 1, 1, 1, 1, 1, 1, 1, 1, 1, 1, 1, 4 ),
 ( 0.000000000000000000, 1.000000000000000000 ),
 ( -0.008481365240538999567, 0.000000000000000000, 0.03418499052141999589, 0.06705543243986999968, 0.09609225505224000541, 0.1212689627326999919, 0.1445858237144000136, 0.1683350686350000014, 0.1924153997444999764, 0.2163475385441999965, 0.2400901845063000140, 0.2638872993326000227, 0.2883641926465000394, 0.3138739111173999841, 0.3400736664824999811, 0.3669224033080000225, 0.3952263667259999780, 0.4258975072560999831, 0.4597904367344000098, 0.4962938553987999990, 0.5331571951194999937, 0.5680640359449000698, 0.5998794348263000176, 0.6292819723868000592, 0.6571102200006999627, 0.6841458463841999516, 0.7104758728877998974, 0.7357936615436999617, 0.7602320418247999756, 0.7841586104491999887, 0.8079717864086000123, 0.8319769714029000562, 0.8557114603086999338, 0.8789861807339000022, 0.9040973669459999584, 0.9330567862467999962, 0.9658526712421000582, 1.000000000000000000, 1.007721702948999987 ),
 .UNSPECIFIED. ) 
 GEOMETRIC_REPRESENTATION_ITEM ( )  RATIONAL_B_SPLINE_SURFACE ( (
 ( 1.236577362560999926, 1.236577362560999926, 1.236577362560999926, 1.236577362560999926, 1.236577362560999926, 1.236577362560999926, 1.236577362560999926, 1.236577362560999926, 1.236577362560999926, 1.236577362560999926, 1.236577362560999926, 1.236577362560999926, 1.236577362560999926, 1.236577362560999926, 1.236577362560999926, 1.236577362560999926, 1.236577362560999926, 1.236577362560999926, 1.236577362560999926, 1.236577362560999926, 1.236577362560999926, 1.236577362560999926, 1.236577362560999926, 1.236577362560999926, 1.236577362560999926, 1.236577362560999926, 1.236577362560999926, 1.236577362560999926, 1.236577362560999926, 1.236577362560999926, 1.236577362560999926, 1.236577362560999926, 1.236577362560999926, 1.236577362560999926, 1.236577362560999926, 1.236577362560999926, 1.236577362560999926, 1.236577362560999926, 1.236577362560999926, 1.236577362560999926, 1.236577362560999926),
 ( 0.9211408791463999712, 0.9211408791463999712, 0.9211408791463999712, 0.9211408791463999712, 0.9211408791463999712, 0.9211408791463999712, 0.9211408791463999712, 0.9211408791463999712, 0.9211408791463999712, 0.9211408791463999712, 0.9211408791463999712, 0.9211408791463999712, 0.9211408791463999712, 0.9211408791463999712, 0.9211408791463999712, 0.9211408791463999712, 0.9211408791463999712, 0.9211408791463999712, 0.9211408791463999712, 0.9211408791463999712, 0.9211408791463999712, 0.9211408791463999712, 0.9211408791463999712, 0.9211408791463999712, 0.9211408791463999712, 0.9211408791463999712, 0.9211408791463999712, 0.9211408791463999712, 0.9211408791463999712, 0.9211408791463999712, 0.9211408791463999712, 0.9211408791463999712, 0.9211408791463999712, 0.9211408791463999712, 0.9211408791463999712, 0.9211408791463999712, 0.9211408791463999712, 0.9211408791463999712, 0.9211408791463999712, 0.9211408791463999712, 0.9211408791463999712),
 ( 0.9211408791463999712, 0.9211408791463999712, 0.9211408791463999712, 0.9211408791463999712, 0.9211408791463999712, 0.9211408791463999712, 0.9211408791463999712, 0.9211408791463999712, 0.9211408791463999712, 0.9211408791463999712, 0.9211408791463999712, 0.9211408791463999712, 0.9211408791463999712, 0.9211408791463999712, 0.9211408791463999712, 0.9211408791463999712, 0.9211408791463999712, 0.9211408791463999712, 0.9211408791463999712, 0.9211408791463999712, 0.9211408791463999712, 0.9211408791463999712, 0.9211408791463999712, 0.9211408791463999712, 0.9211408791463999712, 0.9211408791463999712, 0.9211408791463999712, 0.9211408791463999712, 0.9211408791463999712, 0.9211408791463999712, 0.9211408791463999712, 0.9211408791463999712, 0.9211408791463999712, 0.9211408791463999712, 0.9211408791463999712, 0.9211408791463999712, 0.9211408791463999712, 0.9211408791463999712, 0.9211408791463999712, 0.9211408791463999712, 0.9211408791463999712),
 ( 1.236577362560999926, 1.236577362560999926, 1.236577362560999926, 1.236577362560999926, 1.236577362560999926, 1.236577362560999926, 1.236577362560999926, 1.236577362560999926, 1.236577362560999926, 1.236577362560999926, 1.236577362560999926, 1.236577362560999926, 1.236577362560999926, 1.236577362560999926, 1.236577362560999926, 1.236577362560999926, 1.236577362560999926, 1.236577362560999926, 1.236577362560999926, 1.236577362560999926, 1.236577362560999926, 1.236577362560999926, 1.236577362560999926, 1.236577362560999926, 1.236577362560999926, 1.236577362560999926, 1.236577362560999926, 1.236577362560999926, 1.236577362560999926, 1.236577362560999926, 1.236577362560999926, 1.236577362560999926, 1.236577362560999926, 1.236577362560999926, 1.236577362560999926, 1.236577362560999926, 1.236577362560999926, 1.236577362560999926, 1.236577362560999926, 1.236577362560999926, 1.236577362560999926) ) ) 
 REPRESENTATION_ITEM ( '' )  SURFACE ( )  );
#3999 = CARTESIAN_POINT ( 'NONE',  ( -10.00000000000000000, 2.500000000000000000, -272.5000000000000000 ) ) ;
#4000 = EDGE_CURVE ( 'NONE', #10444, #1207, #4176, .T. ) ;
#4001 = ORIENTED_EDGE ( 'NONE', *, *, #5951, .F. ) ;
#4002 = CARTESIAN_POINT ( 'NONE',  ( 10.00000000000000000, -2.500000000000000000, -317.5000000000000000 ) ) ;
#4003 = VERTEX_POINT ( 'NONE', #2821 ) ;
#4004 = CARTESIAN_POINT ( 'NONE',  ( -14.21175436428723771, -5.188485551603381651, 315.0000000000000000 ) ) ;
#4005 = CARTESIAN_POINT ( 'NONE',  ( 15.69672544750998888, -7.226176219113002119, -302.4229045757450081 ) ) ;
#4006 = DIRECTION ( 'NONE',  ( -4.096342363382135256E-11, 1.000000000000000000, -4.416507306988328157E-12 ) ) ;
#4007 =( REPRESENTATION_RELATIONSHIP ('NONE','NONE', #8468, #7381 ) REPRESENTATION_RELATIONSHIP_WITH_TRANSFORMATION ( #9087 )SHAPE_REPRESENTATION_RELATIONSHIP( ) );
#4008 = DIRECTION ( 'NONE',  ( 0.7172627762233165782, -0.1147078669353000374, 0.6872963080852203532 ) ) ;
#4009 =( NAMED_UNIT ( * ) PLANE_ANGLE_UNIT ( ) SI_UNIT ( $, .RADIAN. ) );
#4010 = CARTESIAN_POINT ( 'NONE',  ( 19.95002954278003315, 1.762942793154997911, -302.9207377450070453 ) ) ;
#4011 = CARTESIAN_POINT ( 'NONE',  ( -41.35482467236749926, -8.000000000000000000, -366.8119992166443808 ) ) ;
#4012 = VERTEX_POINT ( 'NONE', #3627 ) ;
#4013 = CARTESIAN_POINT ( 'NONE',  ( -15.89383674730000173, -3.622219875512000087, -314.8616023057000461 ) ) ;
#4014 = CARTESIAN_POINT ( 'NONE',  ( -2.737737974997910051, -2.627294679320482995, -435.0800218237813510 ) ) ;
#4015 = ORIENTED_EDGE ( 'NONE', *, *, #3777, .F. ) ;
#4016 = CARTESIAN_POINT ( 'NONE',  ( -13.71790339694999439, -8.616951602761004025, 189.9229057364800042 ) ) ;
#4017 = CARTESIAN_POINT ( 'NONE',  ( 8.835721849737728562, 11.22420793802478123, 190.9999999999996589 ) ) ;
#4018 = DIRECTION ( 'NONE',  ( 0.000000000000000000, -1.000000000000000000, 0.000000000000000000 ) ) ;
#4019 = AXIS2_PLACEMENT_3D ( 'NONE', #225, #4359, #5160 ) ;
#4020 = SHAPE_REPRESENTATION ( 'Pivot Pin', ( #2817 ), #2849 ) ;
#4021 = CIRCLE ( 'NONE', #3341, 11.99999961561997885 ) ;
#4022 = CARTESIAN_POINT ( 'NONE',  ( -3.874983216044999956, -9.425407904674999671, 314.8616023057000461 ) ) ;
#4023 = CIRCLE ( 'NONE', #2697, 15.49999999999999467 ) ;
#4024 = CARTESIAN_POINT ( 'NONE',  ( 9.820740202793000861, 9.834836518498999425, 320.0000000000000000 ) ) ;
#4025 = CARTESIAN_POINT ( 'NONE',  ( -24.37035621709999944, -9.500000000000001776, -411.9118794995000030 ) ) ;
#4026 = CARTESIAN_POINT ( 'NONE',  ( -15.56166711177641560, 7.864757419948934292, 319.0000000000005116 ) ) ;
#4027 = CARTESIAN_POINT ( 'NONE',  ( -14.91834191543264154, -4.191152579685455848, -438.6965806410613027 ) ) ;
#4028 = CARTESIAN_POINT ( 'NONE',  ( -72.90663470102438737, -12.00000000000000000, -371.7168990826883714 ) ) ;
#4029 = ORIENTED_EDGE ( 'NONE', *, *, #8616, .T. ) ;
#4030 = CARTESIAN_POINT ( 'NONE',  ( -20.00000000000000000, -4.642018570833219964E-09, -316.5000000000000000 ) ) ;
#4031 = AXIS2_PLACEMENT_3D ( 'NONE', #10563, #85, #6584 ) ;
#4032 = ORIENTED_EDGE ( 'NONE', *, *, #2909, .T. ) ;
#4033 = EDGE_CURVE ( 'NONE', #10001, #4938, #9478, .T. ) ;
#4034 = ORIENTED_EDGE ( 'NONE', *, *, #6814, .F. ) ;
#4035 = CARTESIAN_POINT ( 'NONE',  ( 7.420201433257000545, 2.500000000000000000, -419.8948508258000061 ) ) ;
#4036 = ADVANCED_FACE ( 'NONE', ( #4528 ), #1307, .T. ) ;
#4037 = CARTESIAN_POINT ( 'NONE',  ( 12.45718924559404250, 6.445992642206118006, 315.0000000000000568 ) ) ;
#4038 = SHAPE_DEFINITION_REPRESENTATION ( #467, #1832 ) ;
#4039 = CARTESIAN_POINT ( 'NONE',  ( -19.99999035944999903, 7.277427703818000446E-10, -303.5000000000000000 ) ) ;
#4040 = EDGE_CURVE ( 'NONE', #22, #9921, #9279, .T. ) ;
#4041 = CARTESIAN_POINT ( 'NONE',  ( 16.90887668763000207, -0.2823175147257999673, -315.0848619657999734 ) ) ;
#4042 = CARTESIAN_POINT ( 'NONE',  ( -43.65370867118748777, -2.500000000000000000, -412.6743931307942717 ) ) ;
#4043 = CARTESIAN_POINT ( 'NONE',  ( -6.123887805759949288, -6.692614082003444764, -437.0035920074212186 ) ) ;
#4044 = CARTESIAN_POINT ( 'NONE',  ( 17.04162109443001683, 6.546751591322998109, 318.8802828394900644 ) ) ;
#4045 = CARTESIAN_POINT ( 'NONE',  ( -14.95752314510466086, -6.038563360535726510, -438.5367956719984477 ) ) ;
#4046 = CARTESIAN_POINT ( 'NONE',  ( -1.339600748765887639, -2.618129512416002669, -435.1727200896621639 ) ) ;
#4047 = EDGE_LOOP ( 'NONE', ( #9778, #577, #9554, #9446, #4375 ) ) ;
#4048 = CARTESIAN_POINT ( 'NONE',  ( 20.01656911870001920, 0.3693805509907998053, -316.3802825947000201 ) ) ;
#4049 = CYLINDRICAL_SURFACE ( 'NONE', #4967, 0.9999999999999971134 ) ;
#4050 =( GEOMETRIC_REPRESENTATION_CONTEXT ( 3 ) GLOBAL_UNCERTAINTY_ASSIGNED_CONTEXT ( ( #6573 ) ) GLOBAL_UNIT_ASSIGNED_CONTEXT ( ( #5822, #3307, #10613 ) ) REPRESENTATION_CONTEXT ( 'NONE', 'WORKASPACE' ) );
#4051 = CARTESIAN_POINT ( 'NONE',  ( -14.26294315260000012, -7.573769859179999564, 320.0000000000000000 ) ) ;
#4052 = EDGE_CURVE ( 'NONE', #6958, #5924, #5282, .T. ) ;
#4053 = CARTESIAN_POINT ( 'NONE',  ( -1.157768362637200621, -7.405868988916000539, -434.6424742340107059 ) ) ;
#4054 = PLANE ( 'NONE',  #9090 ) ;
#4055 = CARTESIAN_POINT ( 'NONE',  ( -17.21226690345150701, 1.804990710747427007, -314.5172708043663192 ) ) ;
#4056 = ORIENTED_EDGE ( 'NONE', *, *, #2343, .T. ) ;
#4057 = CARTESIAN_POINT ( 'NONE',  ( 8.037373804805000077, 9.179324345868998591, -315.0000000000001137 ) ) ;
#4058 = ORIENTED_EDGE ( 'NONE', *, *, #2463, .T. ) ;
#4059 = CARTESIAN_POINT ( 'NONE',  ( -8.094664229193854865, 11.44201740537352663, -316.5000000000004547 ) ) ;
#4060 = ORIENTED_EDGE ( 'NONE', *, *, #7192, .F. ) ;
#4061 = CARTESIAN_POINT ( 'NONE',  ( 9.252434838928003558, -11.08696499602999630, -303.6197174156509391 ) ) ;
#4062 = LINE ( 'NONE', #4816, #1710 ) ;
#4063 = DIRECTION ( 'NONE',  ( 0.000000000000000000, -1.000000000000000000, 0.000000000000000000 ) ) ;
#4064 = AXIS2_PLACEMENT_3D ( 'NONE', #5165, #6733, #3657 ) ;
#4065 = CARTESIAN_POINT ( 'NONE',  ( 20.05662131630997536, -0.5622531596958006972, -302.9207377450070453 ) ) ;
#4066 = DIRECTION ( 'NONE',  ( -0.7784864941890657919, 0.000000000000000000, -0.6276613564377032661 ) ) ;
#4067 = VERTEX_POINT ( 'NONE', #7015 ) ;
#4068 = CARTESIAN_POINT ( 'NONE',  ( -17.42228208267999889, -1.444224815522999972, -314.4150829855000211 ) ) ;
#4069 = CARTESIAN_POINT ( 'NONE',  ( -17.34693632642999717, -0.4167404706239999923, 314.6383426456000052 ) ) ;
#4070 = ORIENTED_EDGE ( 'NONE', *, *, #7641, .T. ) ;
#4071 = CARTESIAN_POINT ( 'NONE',  ( -18.87182479219000442, 0.3569112016842001522, 190.0071920248299477 ) ) ;
#4072 = LINE ( 'NONE', #1547, #86 ) ;
#4073 = CARTESIAN_POINT ( 'NONE',  ( 16.25556775813545940, 2.760696635281385092, -314.9999999999999432 ) ) ;
#4074 = DIRECTION ( 'NONE',  ( 0.000000000000000000, -1.000000000000000000, 0.000000000000000000 ) ) ;
#4075 = CARTESIAN_POINT ( 'NONE',  ( -11.89238025184999792, -6.701939844102000166, 315.0848619657999734 ) ) ;
#4076 =( NAMED_UNIT ( * ) SI_UNIT ( $, .STERADIAN. ) SOLID_ANGLE_UNIT ( ) );
#4077 = CARTESIAN_POINT ( 'NONE',  ( 18.53598399141000286, 2.541378258162000137, 320.0000000000000000 ) ) ;
#4078 = CARTESIAN_POINT ( 'NONE',  ( -102.0103468492230547, -2.500000000000000000, -289.6591388711787545 ) ) ;
#4079 = AXIS2_PLACEMENT_3D ( 'NONE', #5746, #6448, #9620 ) ;
#4080 = CARTESIAN_POINT ( 'NONE',  ( -12.96318846091385346, 9.529552999724863582, 319.0000000000005116 ) ) ;
#4081 = CARTESIAN_POINT ( 'NONE',  ( -14.91670604979136883, -4.198290335482643520, -438.7032518645799541 ) ) ;
#4082 = PLANE ( 'NONE',  #9182 ) ;
#4083 = ORIENTED_EDGE ( 'NONE', *, *, #8906, .T. ) ;
#4084 = CARTESIAN_POINT ( 'NONE',  ( -14.79012398733999945, 1.483731117707000058, -285.0000000000000000 ) ) ;
#4085 = SHAPE_REPRESENTATION ( 'Upper Cutting Blade', ( #2817 ), #7989 ) ;
#4086 = ORIENTED_EDGE ( 'NONE', *, *, #457, .F. ) ;
#4087 = VECTOR ( 'NONE', #1922, 1000.000000000000114 ) ;
#4088 = CARTESIAN_POINT ( 'NONE',  ( -76.59645255500944927, -12.00000000000000000, -359.7738992834581495 ) ) ;
#4089 = CARTESIAN_POINT ( 'NONE',  ( 13.98386538276810498, 5.376986245914816109, 315.0000000000000568 ) ) ;
#4090 = CARTESIAN_POINT ( 'NONE',  ( 12.98706127646999953, 6.788989183774999603, -315.0000000000000000 ) ) ;
#4091 = CARTESIAN_POINT ( 'NONE',  ( -46.74071243419621169, -7.500000000000000888, -414.3237589990241077 ) ) ;
#4092 = DIRECTION ( 'NONE',  ( 0.4806425702415767498, 0.000000000000000000, -0.8769165978994644117 ) ) ;
#4093 = CARTESIAN_POINT ( 'NONE',  ( -1.582650547086741799, -7.339339277715000165, -435.1382983596024019 ) ) ;
#4094 = FACE_OUTER_BOUND ( 'NONE', #7595, .T. ) ;
#4095 = CARTESIAN_POINT ( 'NONE',  ( -0.09974927406761666115, -2.336362244183999959, -434.1289336018982112 ) ) ;
#4096 = VERTEX_POINT ( 'NONE', #454 ) ;
#4097 = CARTESIAN_POINT ( 'NONE',  ( -3.772811979575000141, 12.36790329786001763, -317.0792622552969533 ) ) ;
#4098 = PRODUCT_RELATED_PRODUCT_CATEGORY ( 'part', '', ( #1232 ) ) ;
#4099 = DIRECTION ( 'NONE',  ( 0.000000000000000000, 0.000000000000000000, 1.000000000000000000 ) ) ;
#4100 = PLANE ( 'NONE',  #2371 ) ;
#4101 = CARTESIAN_POINT ( 'NONE',  ( -1.439479021682663618, -7.379377528465000502, -434.7575680031760044 ) ) ;
#4102 = UNCERTAINTY_MEASURE_WITH_UNIT (LENGTH_MEASURE( 1.000000000000000082E-05 ), #6052, 'distance_accuracy_value', 'NONE');
#4103 = FACE_OUTER_BOUND ( 'NONE', #80, .T. ) ;
#4104 = CARTESIAN_POINT ( 'NONE',  ( 16.24410010525431503, -2.791089382272744501, -315.0000000000000568 ) ) ;
#4105 = ORIENTED_EDGE ( 'NONE', *, *, #2596, .T. ) ;
#4106 = CARTESIAN_POINT ( 'NONE',  ( 17.50000000000125056, 1.338989683019597976E-14, -314.4963898845653034 ) ) ;
#4107 = VERTEX_POINT ( 'NONE', #1200 ) ;
#4108 = CARTESIAN_POINT ( 'NONE',  ( 7.617198281494000689, 10.53565010756000042, -317.5000000000000000 ) ) ;
#4109 = ORIENTED_EDGE ( 'NONE', *, *, #3912, .T. ) ;
#4110 = DIRECTION ( 'NONE',  ( -0.3420201433256988555, 0.000000000000000000, 0.9396926207858975477 ) ) ;
#4111 = AXIS2_PLACEMENT_3D ( 'NONE', #8207, #8043, #5729 ) ;
#4112 = AXIS2_PLACEMENT_3D ( 'NONE', #7560, #1000, #5028 ) ;
#4113 = EDGE_CURVE ( 'NONE', #4804, #9921, #666, .T. ) ;
#4114 = DIRECTION ( 'NONE',  ( 0.000000000000000000, -1.000000000000000000, 0.000000000000000000 ) ) ;
#4115 = EDGE_CURVE ( 'NONE', #3262, #7113, #1602, .T. ) ;
#4116 = CARTESIAN_POINT ( 'NONE',  ( 13.57573464316000056, -3.225916527208000151, 315.0000000000000000 ) ) ;
#4117 = VECTOR ( 'NONE', #3879, 1000.000000000000000 ) ;
#4118 = CARTESIAN_POINT ( 'NONE',  ( 14.92452513360000310, 8.330674305060012941, -303.6197174156509391 ) ) ;
#4119 = CARTESIAN_POINT ( 'NONE',  ( -46.74071243419000155, -2.500000000000000000, -414.3237589990000629 ) ) ;
#4120 = ORIENTED_EDGE ( 'NONE', *, *, #6677, .T. ) ;
#4121 = CARTESIAN_POINT ( 'NONE',  ( -17.34089965840999881, -0.6440164457022999889, -314.6383426456000052 ) ) ;
#4122 = ADVANCED_FACE ( 'NONE', ( #4755 ), #1358, .T. ) ;
#4123 = DIRECTION ( 'NONE',  ( 0.9712267471052594692, 0.000000000000000000, 0.2381566831044984456 ) ) ;
#4124 = ORIENTED_EDGE ( 'NONE', *, *, #7586, .F. ) ;
#4125 = CARTESIAN_POINT ( 'NONE',  ( 14.87873868498998498, -8.458320990069003287, 190.4207385301700128 ) ) ;
#4126 = CARTESIAN_POINT ( 'NONE',  ( -17.50000000000107292, -0.7437989020622546299, -315.0000000000001137 ) ) ;
#4127 = CARTESIAN_POINT ( 'NONE',  ( 13.67659370612792280, 5.618803873927791237, -315.0000000000000000 ) ) ;
#4128 = EDGE_CURVE ( 'NONE', #289, #1322, #10491, .T. ) ;
#4129 = DIRECTION ( 'NONE',  ( 1.000000000000000000, 0.000000000000000000, 0.000000000000000000 ) ) ;
#4130 = AXIS2_PLACEMENT_3D ( 'NONE', #8785, #1428, #4714 ) ;
#4131 = CARTESIAN_POINT ( 'NONE',  ( 6.488017178959999853, -9.182784307579000327, 314.6383426456000052 ) ) ;
#4132 = CARTESIAN_POINT ( 'NONE',  ( 16.69571944143998365, -6.308604365468005071, 320.0770942683900557 ) ) ;
#4133 = CARTESIAN_POINT ( 'NONE',  ( -27.18445350464674348, -2.500000000000000000, -447.5567201875090291 ) ) ;
#4134 = CARTESIAN_POINT ( 'NONE',  ( 17.13182678275000370, -0.2945984483948000388, 314.8616023057000461 ) ) ;
#4135 = AXIS2_PLACEMENT_3D ( 'NONE', #5568, #3964, #3215 ) ;
#4136 = ORIENTED_EDGE ( 'NONE', *, *, #3365, .F. ) ;
#4137 = CARTESIAN_POINT ( 'NONE',  ( 18.18198898035900157, -5.227591177500494624, 190.9999999999995737 ) ) ;
#4138 = STYLED_ITEM ( 'NONE', ( #1405 ), #1695 ) ;
#4139 = ORIENTED_EDGE ( 'NONE', *, *, #2343, .F. ) ;
#4140 = ADVANCED_FACE ( 'NONE', ( #8135 ), #5544, .T. ) ;
#4141 = CARTESIAN_POINT ( 'NONE',  ( -2.301732014548799388, -2.885986615635997676, -436.1194574627488691 ) ) ;
#4142 = DIRECTION ( 'NONE',  ( 0.000000000000000000, -1.000000000000000000, 0.000000000000000000 ) ) ;
#4143 = CARTESIAN_POINT ( 'NONE',  ( -14.98500449093754483, -5.000000000000000000, -438.4247239981262396 ) ) ;
#4144 = VECTOR ( 'NONE', #7013, 999.9999999999998863 ) ;
#4145 = CARTESIAN_POINT ( 'NONE',  ( -2.001531325394999783, -11.45199047667999892, -302.5000000000000000 ) ) ;
#4146 = LINE ( 'NONE', #10537, #3509 ) ;
#4147 = APPLICATION_CONTEXT ( 'automotive_design' ) ;
#4148 = CARTESIAN_POINT ( 'NONE',  ( -5.884114491779969036, -6.726235514389329317, -436.9226096605755174 ) ) ;
#4149 = DIRECTION ( 'NONE',  ( 0.000000000000000000, -1.000000000000000000, 0.000000000000000000 ) ) ;
#4150 = CARTESIAN_POINT ( 'NONE',  ( 14.79012398733999767, 1.483731117707002278, -284.9999999999999432 ) ) ;
#4151 = ORIENTED_EDGE ( 'NONE', *, *, #5879, .F. ) ;
#4152 = CARTESIAN_POINT ( 'NONE',  ( -19.97263891460998764, -0.5563097477957001935, -316.3802825947000201 ) ) ;
#4153 = ADVANCED_FACE ( 'NONE', ( #1415, #2335 ), #6356, .F. ) ;
#4154 = CARTESIAN_POINT ( 'NONE',  ( 0.6600210488075000104, -11.51366633668999917, 320.0000000000000000 ) ) ;
#4155 = CARTESIAN_POINT ( 'NONE',  ( -0.4121893489828823420, -7.508048508167998847, -434.4353525244472394 ) ) ;
#4156 = AXIS2_PLACEMENT_3D ( 'NONE', #2853, #8692, #594 ) ;
#4157 = CARTESIAN_POINT ( 'NONE',  ( 1.399293614871181202, -7.500000000000000000, -408.6664516090914390 ) ) ;
#4158 = CARTESIAN_POINT ( 'NONE',  ( 2.545630254023275807, -9.391959925330706227, -314.9999999999999432 ) ) ;
#4159 = ORIENTED_EDGE ( 'NONE', *, *, #5744, .T. ) ;
#4160 = CARTESIAN_POINT ( 'NONE',  ( 17.42734739651272946, -0.9144542625322006346, -314.5039539236788642 ) ) ;
#4161 = VERTEX_POINT ( 'NONE', #3026 ) ;
#4162 = DIRECTION ( 'NONE',  ( 0.000000000000000000, -1.000000000000000000, 0.000000000000000000 ) ) ;
#4163 = ORIENTED_EDGE ( 'NONE', *, *, #2998, .F. ) ;
#4164 = CARTESIAN_POINT ( 'NONE',  ( -18.53523119387001117, -4.742105934366003694, -303.6197174156509391 ) ) ;
#4165 = EDGE_CURVE ( 'NONE', #5909, #514, #1425, .T. ) ;
#4166 = CARTESIAN_POINT ( 'NONE',  ( -16.06911929583999310, -5.954958506906000260, -317.4928077629770087 ) ) ;
#4167 = CARTESIAN_POINT ( 'NONE',  ( -5.399293614865643853, -2.500000000000000000, -410.3335483908228980 ) ) ;
#4168 =( LENGTH_UNIT ( ) NAMED_UNIT ( * ) SI_UNIT ( .MILLI., .METRE. ) );
#4169 = EDGE_CURVE ( 'NONE', #7605, #1418, #6411, .T. ) ;
#4170 = CARTESIAN_POINT ( 'NONE',  ( -13.93620031452002728, 8.972937827676991773, -303.6197174156509391 ) ) ;
#4171 = FACE_OUTER_BOUND ( 'NONE', #1691, .T. ) ;
#4172 = VERTEX_POINT ( 'NONE', #8772 ) ;
#4173 = DIRECTION ( 'NONE',  ( 0.8820010751365675583, 0.000000000000000000, 0.4712473909295827323 ) ) ;
#4174 = EDGE_CURVE ( 'NONE', #5957, #5389, #7940, .T. ) ;
#4175 = DIRECTION ( 'NONE',  ( 0.000000000000000000, -1.000000000000000000, 0.000000000000000000 ) ) ;
#4176 = CIRCLE ( 'NONE', #5196, 0.5000000000000074385 ) ;
#4177 = ORIENTED_EDGE ( 'NONE', *, *, #4224, .F. ) ;
#4178 = CARTESIAN_POINT ( 'NONE',  ( -0.7143903809592004883, -12.58977731883000750, 190.4207385301700128 ) ) ;
#4179 = CARTESIAN_POINT ( 'NONE',  ( -28.19723202891387359, -9.000000000000001776, -417.3534541501846888 ) ) ;
#4180 = CYLINDRICAL_SURFACE ( 'NONE', #7883, 5.000000000000004441 ) ;
#4181 = CYLINDRICAL_SURFACE ( 'NONE', #3426, 3.500000000000020428 ) ;
#4182 = CARTESIAN_POINT ( 'NONE',  ( 0.7143903809590995690, 12.58977731883000750, 190.4207385301700128 ) ) ;
#4183 = AXIS2_PLACEMENT_3D ( 'NONE', #1362, #7122, #7915 ) ;
#4184 = CARTESIAN_POINT ( 'NONE',  ( 17.34500932694999875, -0.6070218422356999932, 314.6383426456000052 ) ) ;
#4185 = ADVANCED_FACE ( 'NONE', ( #1583 ), #5603, .T. ) ;
#4186 = CARTESIAN_POINT ( 'NONE',  ( -33.34106825788445150, -7.500000000000000000, -439.6766126514281154 ) ) ;
#4187 = CARTESIAN_POINT ( 'NONE',  ( 19.56036991370999800, 0.5261966905397996719, 320.0770942683900557 ) ) ;
#4188 = DIRECTION ( 'NONE',  ( -0.000000000000000000, 1.000000000000000000, 0.000000000000000000 ) ) ;
#4189 = CARTESIAN_POINT ( 'NONE',  ( 5.255569329967310743, 12.07344867603089611, -303.5000000000000000 ) ) ;
#4190 = CARTESIAN_POINT ( 'NONE',  ( 14.23799507159000122, 5.083276007328000112, 315.0848619657999734 ) ) ;
#4191 = VERTEX_POINT ( 'NONE', #8024 ) ;
#4192 = DIRECTION ( 'NONE',  ( 0.2756373558169616378, 0.000000000000000000, -0.9612616959383295523 ) ) ;
#4193 = ORIENTED_EDGE ( 'NONE', *, *, #6151, .F. ) ;
#4194 = ORIENTED_EDGE ( 'NONE', *, *, #4113, .F. ) ;
#4195 = AXIS2_PLACEMENT_3D ( 'NONE', #8562, #6046, #1314 ) ;
#4196 = AXIS2_PLACEMENT_3D ( 'NONE', #6904, #8452, #10172 ) ;
#4197 = CARTESIAN_POINT ( 'NONE',  ( -5.632814578931469640, -3.468398185772000097, -436.9796822201103055 ) ) ;
#4198 = CARTESIAN_POINT ( 'NONE',  ( -11.65165375873240450, 6.897932327036405020, 315.0000000000000568 ) ) ;
#4199 = CARTESIAN_POINT ( 'NONE',  ( 7.006889269069000115, -6.844138725329000472, -285.0000000000000000 ) ) ;
#4200 = AXIS2_PLACEMENT_3D ( 'NONE', #4427, #1803, #2765 ) ;
#4201 = ORIENTED_EDGE ( 'NONE', *, *, #457, .T. ) ;
#4202 = CARTESIAN_POINT ( 'NONE',  ( -34.39269738225353024, -7.500000000000000000, -407.7262955260336525 ) ) ;
#4203 = CLOSED_SHELL ( 'NONE', ( #5231, #913, #9150, #8034, #1137, #3331, #1125, #4486, #6503, #6209, #3855, #3108, #8518, #9851, #2256, #8303, #3101, #248, #9186, #9553, #10308, #2228, #6474, #2215 ) ) ;
#4204 = DIRECTION ( 'NONE',  ( 0.000000000000000000, 1.000000000000000000, -0.000000000000000000 ) ) ;
#4205 = DIRECTION ( 'NONE',  ( -1.318389841742372130E-13, 1.000000000000000000, -2.220446049250311061E-13 ) ) ;
#4206 =( NAMED_UNIT ( * ) SI_UNIT ( $, .STERADIAN. ) SOLID_ANGLE_UNIT ( ) );
#4207 = CARTESIAN_POINT ( 'NONE',  ( 15.00000000000071587, 0.4945770392355663403, -284.9999999999999432 ) ) ;
#4208 = CARTESIAN_POINT ( 'NONE',  ( 17.49999999954662044, -9.625715914672042649E-06, 190.0000000000000000 ) ) ;
#4209 = CARTESIAN_POINT ( 'NONE',  ( 3.356563794682998925, 12.33103673683000423, -316.3802825947000201 ) ) ;
#4210 = CIRCLE ( 'NONE', #10212, 4.000000000000009770 ) ;
#4211 = CARTESIAN_POINT ( 'NONE',  ( 7.487150678296747408, -5.639452090671036366, -525.6770824513915841 ) ) ;
#4212 = CARTESIAN_POINT ( 'NONE',  ( -2.000000000000000000, -2.500000000000000000, -409.5000000000000568 ) ) ;
#4213 = CARTESIAN_POINT ( 'NONE',  ( 8.673912564134326431, -8.158689640371338925, -315.0000000000000000 ) ) ;
#4214 = ORIENTED_EDGE ( 'NONE', *, *, #10035, .T. ) ;
#4215 = CARTESIAN_POINT ( 'NONE',  ( -4.557748955467412877, -9.652551271539406841, -314.5171779026347281 ) ) ;
#4216 = EDGE_LOOP ( 'NONE', ( #2659, #3329 ) ) ;
#4217 = DIRECTION ( 'NONE',  ( -0.2951854283188045658, 0.000000000000000000, 0.9554399839384175586 ) ) ;
#4218 = ORIENTED_EDGE ( 'NONE', *, *, #6330, .T. ) ;
#4219 = CARTESIAN_POINT ( 'NONE',  ( -10.53744240725999681, -10.62869657088999986, -303.6197174156509391 ) ) ;
#4220 = CARTESIAN_POINT ( 'NONE',  ( -1.546121016139999638, -11.35842264293001591, -317.4928077629770087 ) ) ;
#4221 = LINE ( 'NONE', #8295, #5908 ) ;
#4222 =( NAMED_UNIT ( * ) PLANE_ANGLE_UNIT ( ) SI_UNIT ( $, .RADIAN. ) );
#4223 =( GEOMETRIC_REPRESENTATION_CONTEXT ( 3 ) GLOBAL_UNCERTAINTY_ASSIGNED_CONTEXT ( ( #5061 ) ) GLOBAL_UNIT_ASSIGNED_CONTEXT ( ( #9060, #9759, #1596 ) ) REPRESENTATION_CONTEXT ( 'NONE', 'WORKASPACE' ) );
#4224 = EDGE_CURVE ( 'NONE', #7676, #245, #3617, .T. ) ;
#4225 = CARTESIAN_POINT ( 'NONE',  ( 6.686361683900003072, 11.78513185998999546, -303.6197174156509391 ) ) ;
#4226 = CARTESIAN_POINT ( 'NONE',  ( 19.99998650234378417, -8.894530540522598959E-07, -302.9142199863263158 ) ) ;
#4227 = VERTEX_POINT ( 'NONE', #6168 ) ;
#4228 = CARTESIAN_POINT ( 'NONE',  ( -16.75097866579000083, -2.074182492207000461, -314.8616023057000461 ) ) ;
#4229 = CARTESIAN_POINT ( 'NONE',  ( -14.96977070983867009, -7.500000000000000888, -385.2505660326773409 ) ) ;
#4230 = ORIENTED_EDGE ( 'NONE', *, *, #7181, .T. ) ;
#4231 = CARTESIAN_POINT ( 'NONE',  ( 15.66663193639001506, -7.880331994043005217, 190.4207385301700128 ) ) ;
#4232 = CARTESIAN_POINT ( 'NONE',  ( -12.98706127646999953, -6.788989183774999603, -314.4944826805095772 ) ) ;
#4233 = CARTESIAN_POINT ( 'NONE',  ( 13.37774034208871399, 5.841704189632139332, -314.9999999999999432 ) ) ;
#4234 = CARTESIAN_POINT ( 'NONE',  ( -46.74071243416547361, -2.500000000000000000, -414.3237589990478114 ) ) ;
#4235 = CARTESIAN_POINT ( 'NONE',  ( 15.65104815535000071, 7.893060908445997725, 190.4207385301700128 ) ) ;
#4236 = CARTESIAN_POINT ( 'NONE',  ( -18.86318716375000193, 0.4770217013004998119, 319.9928079742500131 ) ) ;
#4237 = EDGE_CURVE ( 'NONE', #563, #6747, #5859, .T. ) ;
#4238 = EDGE_CURVE ( 'NONE', #1396, #4540, #1556, .T. ) ;
#4239 = CARTESIAN_POINT ( 'NONE',  ( 17.13090252310000139, 0.3058267005333999977, 314.8616023057000461 ) ) ;
#4240 = DIRECTION ( 'NONE',  ( 0.4712473909295827323, 0.000000000000000000, -0.8820010751365675583 ) ) ;
#4241 = CARTESIAN_POINT ( 'NONE',  ( -6.386114867952997542, -11.42839325896998481, 320.0770942683900557 ) ) ;
#4242 = CARTESIAN_POINT ( 'NONE',  ( -14.91207365418872044, 5.270756744682541850, 314.4999413757458342 ) ) ;
#4243 = CARTESIAN_POINT ( 'NONE',  ( 16.39086977655999888, 2.839079766962000040, 314.8616023057000461 ) ) ;
#4244 = EDGE_LOOP ( 'NONE', ( #9537, #7429, #6772, #5929 ) ) ;
#4245 = CARTESIAN_POINT ( 'NONE',  ( -13.01454326516111237, -9.502166178128929275, 190.9999999999995737 ) ) ;
#4246 = ORIENTED_EDGE ( 'NONE', *, *, #1711, .F. ) ;
#4247 = CARTESIAN_POINT ( 'NONE',  ( 20.04731132535002303, 0.9079451813825001327, 319.5792614743400009 ) ) ;
#4248 = ORIENTED_EDGE ( 'NONE', *, *, #2542, .T. ) ;
#4249 = ADVANCED_FACE ( 'NONE', ( #2468 ), #6604, .F. ) ;
#4250 = ADVANCED_FACE ( 'NONE', ( #8211 ), #3488, .T. ) ;
#4251 = CARTESIAN_POINT ( 'NONE',  ( -10.22024696720772319, -2.952319301924000161, -437.2166397675933354 ) ) ;
#4252 = CARTESIAN_POINT ( 'NONE',  ( -11.74237836840727311, 6.849546447955716211, 315.0000000000000000 ) ) ;
#4253 = CONTEXT_DEPENDENT_SHAPE_REPRESENTATION ( #3038, #3814 ) ;
#4254 = CARTESIAN_POINT ( 'NONE',  ( -7.006889269069000115, -6.844138725329000472, -285.0000000000000000 ) ) ;
#4255 = ORIENTED_EDGE ( 'NONE', *, *, #5245, .F. ) ;
#4256 = CARTESIAN_POINT ( 'NONE',  ( 6.328188536734999481, -10.84734154703999920, -302.5000000000000000 ) ) ;
#4257 =( NAMED_UNIT ( * ) PLANE_ANGLE_UNIT ( ) SI_UNIT ( $, .RADIAN. ) );
#4258 = CARTESIAN_POINT ( 'NONE',  ( -5.872896638795078061, -6.657718028558998746, -436.3255011814985096 ) ) ;
#4259 = EDGE_CURVE ( 'NONE', #471, #6686, #1076, .T. ) ;
#4260 = CARTESIAN_POINT ( 'NONE',  ( 17.22665784523203669, -1.821305572729455813, 314.4999396030180492 ) ) ;
#4261 = CARTESIAN_POINT ( 'NONE',  ( -0.1804022943502615328, -2.368673688186001769, -434.4369549119049339 ) ) ;
#4262 = CARTESIAN_POINT ( 'NONE',  ( 2.381287040813000348E-07, -10.00000001404999850, 190.0000000000000000 ) ) ;
#4263 = VECTOR ( 'NONE', #6948, 1000.000000000000000 ) ;
#4264 = FACE_BOUND ( 'NONE', #9002, .T. ) ;
#4265 = CARTESIAN_POINT ( 'NONE',  ( -34.37192209818999800, 2.500000000000000000, -461.0868123482000556 ) ) ;
#4266 = PLANE ( 'NONE',  #4428 ) ;
#4267 = CARTESIAN_POINT ( 'NONE',  ( -18.99999441908000009, -1.671652456891999947E-07, 319.0000000000000000 ) ) ;
#4268 = CARTESIAN_POINT ( 'NONE',  ( -2.157987297531679616, -9.422522223986293355, -314.9999999999999432 ) ) ;
#4269 = ORIENTED_EDGE ( 'NONE', *, *, #3388, .T. ) ;
#4270 = CARTESIAN_POINT ( 'NONE',  ( 11.51453371961018490, -7.479120141997832150, -314.5676927934670175 ) ) ;
#4271 = LINE ( 'NONE', #7541, #8819 ) ;
#4272 = ORIENTED_EDGE ( 'NONE', *, *, #8378, .F. ) ;
#4273 = CARTESIAN_POINT ( 'NONE',  ( -11.32071836301000012, 9.223563301002998926, -317.5000000000000000 ) ) ;
#4274 = ORIENTED_EDGE ( 'NONE', *, *, #226, .T. ) ;
#4275 = CARTESIAN_POINT ( 'NONE',  ( -14.92452513360000310, -8.330674305060012941, -303.6197174156509391 ) ) ;
#4276 = CARTESIAN_POINT ( 'NONE',  ( 7.982667963825995194, -11.03627960042998701, -317.5770954168139610 ) ) ;
#4277 = EDGE_CURVE ( 'NONE', #890, #10001, #3165, .T. ) ;
#4278 = CARTESIAN_POINT ( 'NONE',  ( -16.55686070535999832, 1.955716293870999767, -315.0848619657999734 ) ) ;
#4279 = CARTESIAN_POINT ( 'NONE',  ( 71.03268608925270655, 0.000000000000000000, 22.46903440172015465 ) ) ;
#4280 = CARTESIAN_POINT ( 'NONE',  ( -1.673754838359998498, 12.46646309164999522, -303.6197174156520759 ) ) ;
#4281 = CARTESIAN_POINT ( 'NONE',  ( -64.74703706732441333, -8.000000000000000000, -381.8372235071373666 ) ) ;
#4282 = ORIENTED_EDGE ( 'NONE', *, *, #6151, .T. ) ;
#4283 = CARTESIAN_POINT ( 'NONE',  ( -16.90887668763000207, 0.2823175147257999673, -315.0848619657999734 ) ) ;
#4284 = CARTESIAN_POINT ( 'NONE',  ( -8.922355960362999383, 10.14988298126000110, -302.5000000000000000 ) ) ;
#4285 = ORIENTED_EDGE ( 'NONE', *, *, #7731, .T. ) ;
#4286 = CARTESIAN_POINT ( 'NONE',  ( 12.19509678855998835, -10.00267306739999640, 190.4207385301700128 ) ) ;
#4287 = DIRECTION ( 'NONE',  ( 0.000000000000000000, -1.000000000000000000, 0.000000000000000000 ) ) ;
#4288 = CARTESIAN_POINT ( 'NONE',  ( 12.75178873474798991, 6.273979344207472941, -315.0000000000000000 ) ) ;
#4289 = CARTESIAN_POINT ( 'NONE',  ( 17.70739197152998656, 5.947706840970997888, 190.4207385301700128 ) ) ;
#4290 = CIRCLE ( 'NONE', #3254, 3.499999999999999556 ) ;
#4291 = CARTESIAN_POINT ( 'NONE',  ( 16.28527389671999970, -3.844447514156999812, 314.4150829855000211 ) ) ;
#4292 = FILL_AREA_STYLE ('',( #1212 ) ) ;
#4293 = CARTESIAN_POINT ( 'NONE',  ( -80.50174572377882498, -2.500000000000000000, -340.5254349583379394 ) ) ;
#4294 = CARTESIAN_POINT ( 'NONE',  ( -8.948397653779995409, -10.74758637870000477, 320.0770942683900557 ) ) ;
#4295 = CARTESIAN_POINT ( 'NONE',  ( -13.64750600793954227, 6.290789886748213711, 314.4999418822394546 ) ) ;
#4296 =( LENGTH_UNIT ( ) NAMED_UNIT ( * ) SI_UNIT ( .MILLI., .METRE. ) );
#4297 = CARTESIAN_POINT ( 'NONE',  ( 14.67553856548000013, 5.592168771406000438, 314.4150829855000211 ) ) ;
#4298 = ORIENTED_EDGE ( 'NONE', *, *, #432, .T. ) ;
#4299 = CARTESIAN_POINT ( 'NONE',  ( 19.99997381626590709, -0.3203551279404398544, 190.9999999999995737 ) ) ;
#4300 = CARTESIAN_POINT ( 'NONE',  ( 19.97284365803998796, -0.5561741493802002667, 318.8802828394900644 ) ) ;
#4301 = AXIS2_PLACEMENT_3D ( 'NONE', #4143, #117, #8429 ) ;
#4302 = CARTESIAN_POINT ( 'NONE',  ( -2.575517268146169325, -3.018520364412999868, -435.4821344709343975 ) ) ;
#4303 = AXIS2_PLACEMENT_3D ( 'NONE', #3158, #8905, #8793 ) ;
#4304 = CARTESIAN_POINT ( 'NONE',  ( -6.369677570987301252, 8.818560138237836910, 315.0000000000000000 ) ) ;
#4305 = LINE ( 'NONE', #9088, #4970 ) ;
#4306 = ORIENTED_EDGE ( 'NONE', *, *, #5162, .T. ) ;
#4307 = DIRECTION ( 'NONE',  ( 0.000000000000000000, 1.000000000000000000, 0.000000000000000000 ) ) ;
#4308 = ADVANCED_FACE ( 'NONE', ( #2363 ), #5629, .T. ) ;
#4309 = CARTESIAN_POINT ( 'NONE',  ( -1.120069929747936399, -7.393642214682999203, -435.7161955804480726 ) ) ;
#4310 = CARTESIAN_POINT ( 'NONE',  ( -16.68824139745838409, 1.819223930145250856, -315.0000000000000000 ) ) ;
#4311 = CYLINDRICAL_SURFACE ( 'NONE', #8417, 12.49999999999999822 ) ;
#4312 = DIRECTION ( 'NONE',  ( -0.000000000000000000, 1.000000000000000000, 0.000000000000000000 ) ) ;
#4313 = PLANE ( 'NONE',  #2173 ) ;
#4314 = CARTESIAN_POINT ( 'NONE',  ( 8.329446316317595134, -4.252668635446108070, -525.7144557534204523 ) ) ;
#4315 = EDGE_CURVE ( 'NONE', #3465, #8821, #8795, .T. ) ;
#4316 = DIRECTION ( 'NONE',  ( 0.000000000000000000, 1.000000000000000000, 0.000000000000000000 ) ) ;
#4317 = UNCERTAINTY_MEASURE_WITH_UNIT (LENGTH_MEASURE( 1.000000000000000082E-05 ), #1657, 'distance_accuracy_value', 'NONE');
#4318 = CARTESIAN_POINT ( 'NONE',  ( -63.11273421720001409, 2.500000000000000000, -415.2750182148000135 ) ) ;
#4319 = EDGE_CURVE ( 'NONE', #6718, #1530, #1927, .T. ) ;
#4320 = CARTESIAN_POINT ( 'NONE',  ( 13.98368610735813888, -5.377133503752140165, -315.0000000000000568 ) ) ;
#4321 = EDGE_LOOP ( 'NONE', ( #6540, #7792, #8836, #8997 ) ) ;
#4322 = LINE ( 'NONE', #10068, #7974 ) ;
#4323 = CARTESIAN_POINT ( 'NONE',  ( -14.93376631645305253, -8.332910267862528642, -316.5000000000004547 ) ) ;
#4324 = ORIENTED_EDGE ( 'NONE', *, *, #5348, .F. ) ;
#4325 = CARTESIAN_POINT ( 'NONE',  ( -27.98005464532998232, -7.500000000000000888, -417.3300389808354680 ) ) ;
#4326 = ORIENTED_EDGE ( 'NONE', *, *, #8377, .F. ) ;
#4327 = DIRECTION ( 'NONE',  ( 0.1071946444232954182, 0.000000000000000000, -0.9942380540931651245 ) ) ;
#4328 = CARTESIAN_POINT ( 'NONE',  ( 6.660995095996002924, -11.36691212455000333, -317.5770954168139610 ) ) ;
#4329 = CARTESIAN_POINT ( 'NONE',  ( -17.57673583306999632, -0.3313182897943000582, -314.4150829855000211 ) ) ;
#4330 = CARTESIAN_POINT ( 'NONE',  ( -20.01694242003000568, 0.3416920405409001327, -303.6197174156520759 ) ) ;
#4331 = CARTESIAN_POINT ( 'NONE',  ( 10.32803372116435270, 10.00000000000000178, 314.4999507458385324 ) ) ;
#4332 = VERTEX_POINT ( 'NONE', #9296 ) ;
#4333 = CARTESIAN_POINT ( 'NONE',  ( 8.751711036432999080, -10.20177972100999853, 190.0000000000000000 ) ) ;
#4334 = CARTESIAN_POINT ( 'NONE',  ( -15.28688047792000049, 6.812924772642000804, -302.5000000000000000 ) ) ;
#4335 = ORIENTED_EDGE ( 'NONE', *, *, #3614, .T. ) ;
#4336 = AXIS2_PLACEMENT_3D ( 'NONE', #3622, #6030, #1904 ) ;
#4337 = CARTESIAN_POINT ( 'NONE',  ( 18.24410766404003326, -5.273389473771006308, 190.4207385301700128 ) ) ;
#4338 = CARTESIAN_POINT ( 'NONE',  ( -87.43676691142619006, -7.500000000000000000, -348.7659131681800773 ) ) ;
#4339 = CARTESIAN_POINT ( 'NONE',  ( -3.563286991701002382, -11.18699815210999660, -302.5071922382879279 ) ) ;
#4340 = CARTESIAN_POINT ( 'NONE',  ( -17.00602911426001285, 6.582783228486000837, 191.1197171614399792 ) ) ;
#4341 = VECTOR ( 'NONE', #6820, 1000.000000000000000 ) ;
#4342 = CARTESIAN_POINT ( 'NONE',  ( 8.690073206612000334, -8.569658446474999636, 314.6383426456000052 ) ) ;
#4343 = DIRECTION ( 'NONE',  ( 1.000000000000000000, 0.000000000000000000, 0.000000000000000000 ) ) ;
#4344 = PLANE ( 'NONE',  #4501 ) ;
#4345 = VECTOR ( 'NONE', #2416, 1000.000000000000000 ) ;
#4346 = CARTESIAN_POINT ( 'NONE',  ( 18.89077695122000122, -0.08689258194099000465, 319.9928079742500131 ) ) ;
#4347 = CARTESIAN_POINT ( 'NONE',  ( -6.176507045891521663, 9.366274624700933416, 314.4999436549672964 ) ) ;
#4348 = CARTESIAN_POINT ( 'NONE',  ( 10.54003729909880960, 10.63540770771157717, -303.5000000000000000 ) ) ;
#4349 = CARTESIAN_POINT ( 'NONE',  ( 3.903842856253999738, 9.647088721075000706, 314.6383426456000052 ) ) ;
#4350 = VERTEX_POINT ( 'NONE', #5198 ) ;
#4351 = CARTESIAN_POINT ( 'NONE',  ( 19.95972666420564323, -0.9723020053077987557, 190.9999999999995737 ) ) ;
#4352 = CARTESIAN_POINT ( 'NONE',  ( 14.92426358056000701, 8.426786174986000688, 319.5792614743400009 ) ) ;
#4353 =( REPRESENTATION_RELATIONSHIP ('NONE','NONE', #8468, #7381 ) REPRESENTATION_RELATIONSHIP_WITH_TRANSFORMATION ( #6397 )SHAPE_REPRESENTATION_RELATIONSHIP( ) );
#4354 = CARTESIAN_POINT ( 'NONE',  ( -10.00000000000000000, -2.500000000000000000, -272.5000000000000000 ) ) ;
#4355 = CARTESIAN_POINT ( 'NONE',  ( -4.298491262593391760, 9.188587546143761386, 314.9999999999999432 ) ) ;
#4356 = FACE_OUTER_BOUND ( 'NONE', #9247, .T. ) ;
#4357 = EDGE_LOOP ( 'NONE', ( #526, #4825, #1100, #6386 ) ) ;
#4358 = CARTESIAN_POINT ( 'NONE',  ( -0.7348864362710936238, -2.505735680000606536, -434.2545334094357941 ) ) ;
#4359 = DIRECTION ( 'NONE',  ( 0.000000000000000000, 1.000000000000000000, 0.000000000000000000 ) ) ;
#4360 = EDGE_CURVE ( 'NONE', #5864, #1205, #1715, .T. ) ;
#4361 = VECTOR ( 'NONE', #7943, 1000.000000000000000 ) ;
#4362 = CARTESIAN_POINT ( 'NONE',  ( -4.792833739245000224, 11.13811509850999926, 190.0000000000000000 ) ) ;
#4363 = CARTESIAN_POINT ( 'NONE',  ( -14.08970834377950787, 5.290460773273633954, -314.9999999999999432 ) ) ;
#4364 = CARTESIAN_POINT ( 'NONE',  ( 18.85519295008999663, 0.7686777388422003643, 190.0071920248299477 ) ) ;
#4365 = CARTESIAN_POINT ( 'NONE',  ( 10.00000000000000000, -2.500000000000000000, -272.5000000000000000 ) ) ;
#4366 = EDGE_CURVE ( 'NONE', #8504, #4350, #570, .T. ) ;
#4367 = CIRCLE ( 'NONE', #10365, 12.50000000000001243 ) ;
#4368 = FACE_OUTER_BOUND ( 'NONE', #1574, .T. ) ;
#4369 = EDGE_CURVE ( 'NONE', #3371, #3427, #6054, .T. ) ;
#4370 = CARTESIAN_POINT ( 'NONE',  ( 6.127436559474321420, -5.500000000000000000, -524.5233678721955357 ) ) ;
#4371 = DIRECTION ( 'NONE',  ( 0.000000000000000000, -1.000000000000000000, 0.000000000000000000 ) ) ;
#4372 = VERTEX_POINT ( 'NONE', #8263 ) ;
#4373 = CARTESIAN_POINT ( 'NONE',  ( -0.6117794464027001000, 11.39410369034999704, 319.9928079742500131 ) ) ;
#4374 = DIRECTION ( 'NONE',  ( -0.000000000000000000, 1.000000000000000000, 0.000000000000000000 ) ) ;
#4375 = ORIENTED_EDGE ( 'NONE', *, *, #10494, .F. ) ;
#4376 = CARTESIAN_POINT ( 'NONE',  ( -5.500000000000000000, 2.500000000000000000, -409.5000000000000568 ) ) ;
#4377 = ORIENTED_EDGE ( 'NONE', *, *, #6623, .T. ) ;
#4378 = AXIS2_PLACEMENT_3D ( 'NONE', #945, #3312, #5775 ) ;
#4379 =( GEOMETRIC_REPRESENTATION_CONTEXT ( 3 ) GLOBAL_UNCERTAINTY_ASSIGNED_CONTEXT ( ( #5921 ) ) GLOBAL_UNIT_ASSIGNED_CONTEXT ( ( #9665, #1613, #6498 ) ) REPRESENTATION_CONTEXT ( 'NONE', 'WORKASPACE' ) );
#4380 = CARTESIAN_POINT ( 'NONE',  ( -18.86306334786000605, -0.4771235332117997885, -317.4928077629770087 ) ) ;
#4381 = CARTESIAN_POINT ( 'NONE',  ( -8.850998676319990821, -10.04707221382999194, -317.4928077629770087 ) ) ;
#4382 = EDGE_CURVE ( 'NONE', #1301, #1519, #2686, .T. ) ;
#4383 = DIRECTION ( 'NONE',  ( 0.2951854283188049544, 0.000000000000000000, -0.9554399839384174475 ) ) ;
#4384 = CARTESIAN_POINT ( 'NONE',  ( 17.20152651095803975, 1.793788947124328681, -314.5180462286796796 ) ) ;
#4385 = CARTESIAN_POINT ( 'NONE',  ( -7.551285642361038164, -9.031218629016434463, 314.4999459341803458 ) ) ;
#4386 = VERTEX_POINT ( 'NONE', #9189 ) ;
#4387 = CARTESIAN_POINT ( 'NONE',  ( 18.20429351259000228, -3.291556992836000006, 190.0000000000000000 ) ) ;
#4388 = DIRECTION ( 'NONE',  ( -0.9612616959383299964, 0.000000000000000000, -0.2756373558169601945 ) ) ;
#4389 = ORIENTED_EDGE ( 'NONE', *, *, #7954, .T. ) ;
#4390 = CARTESIAN_POINT ( 'NONE',  ( -7.559362580479000115, -11.57734716366000072, 191.1197171614399792 ) ) ;
#4391 = ORIENTED_EDGE ( 'NONE', *, *, #6127, .F. ) ;
#4392 = DIRECTION ( 'NONE',  ( -0.1071946444232947937, 0.000000000000000000, 0.9942380540931651245 ) ) ;
#4393 = CARTESIAN_POINT ( 'NONE',  ( -10.13603924037000326, -9.590552501249007378, -302.5071922382879279 ) ) ;
#4394 = CARTESIAN_POINT ( 'NONE',  ( 17.08426003144000305, 6.624354047749995367, 190.4207385301700128 ) ) ;
#4395 = MECHANICAL_DESIGN_GEOMETRIC_PRESENTATION_REPRESENTATION (  '', ( #3362 ), #9367 ) ;
#4396 = CARTESIAN_POINT ( 'NONE',  ( -0.7192419855824011554, -7.501856097319999250, -434.1639282888053799 ) ) ;
#4397 = CARTESIAN_POINT ( 'NONE',  ( -14.33246323392999422, 7.385748264902002092, -302.5071922382879279 ) ) ;
#4398 = CARTESIAN_POINT ( 'NONE',  ( 6.055260875802999543, -12.00648505189998971, 319.5792614743400009 ) ) ;
#4399 = CARTESIAN_POINT ( 'NONE',  ( 14.57772014836000096, -5.380605385836000565, -314.6383426456000052 ) ) ;
#4400 = CARTESIAN_POINT ( 'NONE',  ( -1.409290114754000012, 9.868237606049000021, 314.6383426456000052 ) ) ;
#4401 = ORIENTED_EDGE ( 'NONE', *, *, #2596, .F. ) ;
#4402 = CARTESIAN_POINT ( 'NONE',  ( 14.93050028969001808, -6.935770771621001529, 190.0071920248299477 ) ) ;
#4403 = ORIENTED_EDGE ( 'NONE', *, *, #8507, .F. ) ;
#4404 = CARTESIAN_POINT ( 'NONE',  ( -12.99935040274999487, 9.597679858163006728, 319.5792614743400009 ) ) ;
#4405 = PRODUCT_DEFINITION_FORMATION_WITH_SPECIFIED_SOURCE ( 'ANY', '', #10331, .NOT_KNOWN. ) ;
#4406 = LINE ( 'NONE', #6164, #3574 ) ;
#4407 = CARTESIAN_POINT ( 'NONE',  ( 1.573733331195987573, 9.469132543440894167, 315.0000000000001137 ) ) ;
#4408 = CARTESIAN_POINT ( 'NONE',  ( 0.000000000000000000, -7.937240849781000307, -284.9999999999999432 ) ) ;
#4409 = CARTESIAN_POINT ( 'NONE',  ( -73.93978370014021095, -7.500000000000000888, -368.3728591389038911 ) ) ;
#4410 = DIRECTION ( 'NONE',  ( -0.1071946444232959594, 0.000000000000000000, 0.9942380540931649024 ) ) ;
#4411 = CARTESIAN_POINT ( 'NONE',  ( 1.604652481465360658, -9.999950686259090560, 314.4999444147077838 ) ) ;
#4412 = PRODUCT_DEFINITION_SHAPE ( 'NONE', 'NONE',  #8229 ) ;
#4413 = CARTESIAN_POINT ( 'NONE',  ( -17.73236801841998300, 3.892024484092002634, 190.0071920248299477 ) ) ;
#4414 = FACE_OUTER_BOUND ( 'NONE', #2889, .T. ) ;
#4415 = DIRECTION ( 'NONE',  ( 0.000000000000000000, -1.000000000000000000, 0.000000000000000000 ) ) ;
#4416 = CARTESIAN_POINT ( 'NONE',  ( 9.378959784071181360, -5.899999999999999467, -525.1866552614185366 ) ) ;
#4417 = PRODUCT_DEFINITION_CONTEXT ( 'detailed design', #1109, 'design' ) ;
#4418 = CARTESIAN_POINT ( 'NONE',  ( -13.49021588649789649, -5.672514732883807476, -439.0878092209056263 ) ) ;
#4419 = ORIENTED_EDGE ( 'NONE', *, *, #181, .T. ) ;
#4420 = VECTOR ( 'NONE', #6286, 1000.000000000000000 ) ;
#4421 = CARTESIAN_POINT ( 'NONE',  ( 18.14104367554000774, 3.149620910056999623, 319.9928079742500131 ) ) ;
#4422 = CARTESIAN_POINT ( 'NONE',  ( -9.195128512800469167, -11.11313767369120775, -316.5000000000004547 ) ) ;
#4423 = CARTESIAN_POINT ( 'NONE',  ( 0.000000000000000000, 0.000000000000000000, 320.0000000000000000 ) ) ;
#4424 = VERTEX_POINT ( 'NONE', #1061 ) ;
#4425 = CARTESIAN_POINT ( 'NONE',  ( -9.022589772749004311, 9.990182113135000819, -317.4928077629770087 ) ) ;
#4426 = CARTESIAN_POINT ( 'NONE',  ( 15.01674827698000314, -8.369013993811000418, -317.0792622552969533 ) ) ;
#4427 = CARTESIAN_POINT ( 'NONE',  ( -1.873948611767810357, -2.500000000000000000, -349.2478646809746579 ) ) ;
#4428 = AXIS2_PLACEMENT_3D ( 'NONE', #6793, #1138, #7535 ) ;
#4429 = ADVANCED_BREP_SHAPE_REPRESENTATION ( '', ( #5374, #2817 ), #2849 ) ;
#4430 = CARTESIAN_POINT ( 'NONE',  ( 17.50000000000000000, 0.000000000000000000, -314.4999343908002629 ) ) ;
#4431 = B_SPLINE_SURFACE_WITH_KNOTS ( 'NONE', 3, 3, ( 
 ( #1503, #3545, #1769, #8322 ),
 ( #3326, #4134, #7622, #7464 ),
 ( #5040, #9298, #2736, #957 ),
 ( #6606, #2523, #7411, #9079 ),
 ( #1826, #6771, #8373, #1929 ),
 ( #10096, #3385, #268, #8423 ),
 ( #6661, #4243, #5091, #5956 ),
 ( #53, #9886, #7515, #6825 ),
 ( #6003, #10045, #1009, #9191 ),
 ( #4190, #159, #5147, #4297 ),
 ( #8213, #3433, #7569, #3492 ),
 ( #5788, #851, #214, #2688 ),
 ( #6712, #9990, #2632, #1716 ),
 ( #4988, #107, #8265, #5895 ),
 ( #904, #9246, #9936, #2574 ),
 ( #1876, #1063, #4349, #5842 ),
 ( #9133, #8623, #1118, #3694 ),
 ( #2991, #6876, #4400, #8572 ),
 ( #6981, #7771, #3643, #5298 ),
 ( #1216, #4494, #6210, #4447 ),
 ( #9346, #9495, #6267, #3593 ),
 ( #9445, #4549, #5200, #5250 ),
 ( #7823, #7087, #415, #1270 ),
 ( #10143, #2135, #1169, #470 ),
 ( #7675, #367, #319, #2786 ),
 ( #7726, #6926, #5402, #8680 ),
 ( #6057, #8473, #10199, #1321 ),
 ( #4604, #3742, #1983, #8524 ),
 ( #2841, #6109, #2031, #7878 ),
 ( #7031, #9546, #10252, #9396 ),
 ( #2888, #6157, #2083, #10303 ),
 ( #5347, #525, #2939, #3798 ),
 ( #10353, #632, #6429, #738 ),
 ( #3261, #8152, #4069, #7994 ) ),
 .UNSPECIFIED., .F., .F., .F.,
 ( 4, 1, 1, 1, 1, 1, 1, 1, 1, 1, 1, 1, 1, 1, 1, 1, 1, 1, 1, 1, 1, 1, 1, 1, 1, 1, 1, 1, 1, 1, 1, 4 ),
 ( 4, 4 ),
 ( -0.01574130609828000224, 0.000000000000000000, 0.03448275862069000164, 0.06896551724138000328, 0.1034482758621000087, 0.1379310344828000023, 0.1724137931033999926, 0.2068965517240999863, 0.2413793103448000077, 0.2758620689655000291, 0.3103448275861999672, 0.3448275862069000164, 0.3793103448276000100, 0.4137931034483000037, 0.4482758620689999973, 0.4827586206897000465, 0.5172413793103000090, 0.5517241379310000582, 0.5862068965516999963, 0.6206896551723999345, 0.6551724137930999836, 0.6896551724138000328, 0.7241379310344999709, 0.7586206896552000201, 0.7931034482758999582, 0.8275862068966000074, 0.8620689655171999144, 0.8965517241379000746, 0.9310344827586000127, 0.9655172413793000619, 1.000000000000000000, 1.014026462982999810 ),
 ( -0.1697239316932999953, 1.169834029081999960 ),
 .UNSPECIFIED. ) ;
#4432 = ORIENTED_EDGE ( 'NONE', *, *, #3251, .F. ) ;
#4433 = CARTESIAN_POINT ( 'NONE',  ( -18.78940217795999956, -1.754852253524999961, 190.0000000000000000 ) ) ;
#4434 = EDGE_CURVE ( 'NONE', #4096, #5868, #10043, .T. ) ;
#4435 = CARTESIAN_POINT ( 'NONE',  ( -1.999999999997229772, -7.500000000000000000, -409.4999999999571969 ) ) ;
#4436 = EDGE_LOOP ( 'NONE', ( #4083, #10241, #3729, #10115 ) ) ;
#4437 = CARTESIAN_POINT ( 'NONE',  ( -6.108404012864005139, -11.90988283206001519, 191.1197171614399792 ) ) ;
#4438 = EDGE_LOOP ( 'NONE', ( #20, #10120, #2959, #9597 ) ) ;
#4439 = CARTESIAN_POINT ( 'NONE',  ( -45.40077937890500692, -8.000000000000000000, -426.7517346751886862 ) ) ;
#4440 = DIRECTION ( 'NONE',  ( 0.9902680687415800209, 0.000000000000000000, 0.1391731009599966873 ) ) ;
#4441 = FACE_OUTER_BOUND ( 'NONE', #5239, .T. ) ;
#4442 = CARTESIAN_POINT ( 'NONE',  ( -0.5256544489318767388, -7.481870571157999805, -434.2361367940509354 ) ) ;
#4443 = EDGE_CURVE ( 'NONE', #189, #8110, #8867, .T. ) ;
#4444 = CARTESIAN_POINT ( 'NONE',  ( 16.85751871341000907, 5.113642021703998175, -302.5071922382879279 ) ) ;
#4445 = CARTESIAN_POINT ( 'NONE',  ( -7.868470208275999411, -11.58296045169998401, 319.5792614743400009 ) ) ;
#4446 = PLANE ( 'NONE',  #2148 ) ;
#4447 = CARTESIAN_POINT ( 'NONE',  ( -6.537559671572000575, 9.400791339334000796, 314.4150829855000211 ) ) ;
#4448 = ORIENTED_EDGE ( 'NONE', *, *, #880, .F. ) ;
#4449 = CARTESIAN_POINT ( 'NONE',  ( -17.02940347669787613, -6.570098831661550953, 190.9999999999995737 ) ) ;
#4450 = CARTESIAN_POINT ( 'NONE',  ( -4.392607225559004291, 12.20457772578000366, 318.8802828394900644 ) ) ;
#4451 = AXIS2_PLACEMENT_3D ( 'NONE', #6520, #2279, #4859 ) ;
#4452 = AXIS2_PLACEMENT_3D ( 'NONE', #9704, #2344, #5613 ) ;
#4453 = DIRECTION ( 'NONE',  ( 0.000000000000000000, -1.000000000000000000, 0.000000000000000000 ) ) ;
#4454 = CARTESIAN_POINT ( 'NONE',  ( -13.94549574055089458, 5.407931305651876741, 315.0000000000001137 ) ) ;
#4455 = DIRECTION ( 'NONE',  ( 0.2728306852451988784, 0.000000000000000000, 0.9620620651437385984 ) ) ;
#4456 = CIRCLE ( 'NONE', #2235, 19.99999999999998934 ) ;
#4457 = CYLINDRICAL_SURFACE ( 'NONE', #10545, 3.500000000000003997 ) ;
#4458 = EDGE_CURVE ( 'NONE', #1542, #10131, #2823, .T. ) ;
#4459 = CARTESIAN_POINT ( 'NONE',  ( -5.631041015997348076, -6.531867497364999053, -436.9792595002378448 ) ) ;
#4460 = CARTESIAN_POINT ( 'NONE',  ( -15.46045765806406891, 3.925441769934806757, -315.0000000000000568 ) ) ;
#4461 = CARTESIAN_POINT ( 'NONE',  ( -1.873948611771682149, -12.50000000000000000, -349.2478646809681777 ) ) ;
#4462 = FACE_BOUND ( 'NONE', #1220, .T. ) ;
#4463 = CARTESIAN_POINT ( 'NONE',  ( 0.2188334844704999949, -11.51755598686999882, -317.5000000000000000 ) ) ;
#4464 = PLANE ( 'NONE',  #5970 ) ;
#4465 = CARTESIAN_POINT ( 'NONE',  ( 15.44313366109816599, -3.946504251847836819, 315.0000000000000568 ) ) ;
#4466 = CARTESIAN_POINT ( 'NONE',  ( 10.50000150490000017, 7.882579085736000302, -314.6383426456000052 ) ) ;
#4467 = VERTEX_POINT ( 'NONE', #2554 ) ;
#4468 = CARTESIAN_POINT ( 'NONE',  ( -12.43797004353999469, 8.540074035031999244, 319.9928079742500131 ) ) ;
#4469 = CARTESIAN_POINT ( 'NONE',  ( -7.865580335751168661, -11.50505378538359125, -316.5000000000004547 ) ) ;
#4470 = DIRECTION ( 'NONE',  ( -0.9712269923486630541, -1.447945891862955814E-12, -0.2381556829751701188 ) ) ;
#4471 = EDGE_LOOP ( 'NONE', ( #4719, #10570, #9184, #1853, #5866, #9685, #776, #5992, #3436, #4965, #7187, #9319, #9698, #9572, #6662, #2281, #7184 ) ) ;
#4472 = CARTESIAN_POINT ( 'NONE',  ( 8.850998676319990821, 10.04707221382999194, -317.4928077629770087 ) ) ;
#4473 = CARTESIAN_POINT ( 'NONE',  ( -19.57077664853002119, 0.3812814288523002082, -317.5770954168139610 ) ) ;
#4474 = CARTESIAN_POINT ( 'NONE',  ( -14.00000000000000000, -2.500000000000000000, -317.5000000000000000 ) ) ;
#4475 = CARTESIAN_POINT ( 'NONE',  ( 16.39561153668567428, 3.420321068896136296, -314.5539561507842450 ) ) ;
#4476 = ORIENTED_EDGE ( 'NONE', *, *, #2723, .F. ) ;
#4477 = CARTESIAN_POINT ( 'NONE',  ( -18.99997815069999874, -0.3119984768183999835, 190.0000000000100044 ) ) ;
#4478 = CARTESIAN_POINT ( 'NONE',  ( 30.17732799123041332, -3.250000000000000444, -426.5781481706914633 ) ) ;
#4479 = ADVANCED_FACE ( 'NONE', ( #4868 ), #1696, .T. ) ;
#4480 = VERTEX_POINT ( 'NONE', #8087 ) ;
#4481 = CARTESIAN_POINT ( 'NONE',  ( -10.00000000000000000, -2.500000000000000000, -317.5000000000000000 ) ) ;
#4482 = EDGE_LOOP ( 'NONE', ( #2393, #4448, #2755, #7916 ) ) ;
#4483 = CARTESIAN_POINT ( 'NONE',  ( -72.90663470102438737, -12.50000000000000000, -368.3168990826883373 ) ) ;
#4484 = DIRECTION ( 'NONE',  ( 0.000000000000000000, 1.000000000000000000, 0.000000000000000000 ) ) ;
#4485 = DIRECTION ( 'NONE',  ( 0.000000000000000000, -1.000000000000000000, 0.000000000000000000 ) ) ;
#4486 = ADVANCED_FACE ( 'NONE', ( #3205 ), #7393, .T. ) ;
#4487 = CARTESIAN_POINT ( 'NONE',  ( -0.6303109507422630653, -7.465267904704998791, -434.3566826232884637 ) ) ;
#4488 =( LENGTH_UNIT ( ) NAMED_UNIT ( * ) SI_UNIT ( .MILLI., .METRE. ) );
#4489 = EDGE_CURVE ( 'NONE', #7069, #6915, #2312, .T. ) ;
#4490 = CARTESIAN_POINT ( 'NONE',  ( -10.11757849520999031, 9.598459870364994373, -302.5071922382879279 ) ) ;
#4491 = CARTESIAN_POINT ( 'NONE',  ( -20.04731132535002303, -0.9079451813825001327, 319.5792614743400009 ) ) ;
#4492 = AXIS2_PLACEMENT_3D ( 'NONE', #906, #7413, #4991 ) ;
#4493 = DIRECTION ( 'NONE',  ( 0.3420201433256991330, 0.000000000000000000, -0.9396926207858973257 ) ) ;
#4494 = CARTESIAN_POINT ( 'NONE',  ( -6.438474686349000997, 8.964777275824999947, 314.8616023057000461 ) ) ;
#4495 = ORIENTED_EDGE ( 'NONE', *, *, #2679, .F. ) ;
#4496 = CARTESIAN_POINT ( 'NONE',  ( -5.890130794754004029, -10.81842929378999330, 190.0071920248299477 ) ) ;
#4497 = VERTEX_POINT ( 'NONE', #4167 ) ;
#4498 = CARTESIAN_POINT ( 'NONE',  ( -0.7615446691253315858, -7.492522473116027371, -434.2738182435463727 ) ) ;
#4499 = DIRECTION ( 'NONE',  ( -0.9902680687415800209, 0.000000000000000000, -0.1391731009599967983 ) ) ;
#4500 = ORIENTED_EDGE ( 'NONE', *, *, #3063, .T. ) ;
#4501 = AXIS2_PLACEMENT_3D ( 'NONE', #3487, #9294, #7407 ) ;
#4502 = DIRECTION ( 'NONE',  ( -1.000000000000000000, 0.000000000000000000, 0.000000000000000000 ) ) ;
#4503 = CARTESIAN_POINT ( 'NONE',  ( 19.00000000000000000, 0.000000000000000000, 319.9999999999899956 ) ) ;
#4504 = DIRECTION ( 'NONE',  ( 0.000000000000000000, 1.000000000000000000, -0.000000000000000000 ) ) ;
#4505 = CARTESIAN_POINT ( 'NONE',  ( -8.586696445213114259, -8.187646113561793726, -314.9999999999999432 ) ) ;
#4506 = DIRECTION ( 'NONE',  ( 0.000000000000000000, 1.000000000000000000, -0.000000000000000000 ) ) ;
#4507 = DIRECTION ( 'NONE',  ( -0.7426245373610013134, 0.000000000000000000, 0.6697079934638370258 ) ) ;
#4508 = CARTESIAN_POINT ( 'NONE',  ( 20.00000000000000000, 7.322330471414334241, -316.5000000000000000 ) ) ;
#4509 = CARTESIAN_POINT ( 'NONE',  ( 8.517086849895166623, 8.210518282650744126, -314.9999999999999432 ) ) ;
#4510 = DIRECTION ( 'NONE',  ( 0.8817975988108817109, 0.000000000000000000, 0.4716280258120411073 ) ) ;
#4511 = CARTESIAN_POINT ( 'NONE',  ( 16.99996037728000076, -1.352915083302999933E-09, -314.9999801883000146 ) ) ;
#4512 = VERTEX_POINT ( 'NONE', #29 ) ;
#4513 = CARTESIAN_POINT ( 'NONE',  ( -16.89340345063000015, -5.253727359668999952, -317.4999999999989768 ) ) ;
#4514 = CARTESIAN_POINT ( 'NONE',  ( -1.999999999997229772, -7.500000000000000000, -409.4999999999571969 ) ) ;
#4515 = AXIS2_PLACEMENT_3D ( 'NONE', #1106, #404, #8516 ) ;
#4516 = DIRECTION ( 'NONE',  ( 1.000000000000000000, 0.000000000000000000, 0.000000000000000000 ) ) ;
#4517 = CARTESIAN_POINT ( 'NONE',  ( 15.88661950543927404, -3.373766516133892335, 315.0000000000000000 ) ) ;
#4518 = CARTESIAN_POINT ( 'NONE',  ( 6.273744347102000241, 8.772995918477999311, -315.0848619657999734 ) ) ;
#4519 = CIRCLE ( 'NONE', #8469, 3.500000000000005773 ) ;
#4520 = CARTESIAN_POINT ( 'NONE',  ( -17.50000000000000000, 1.896400240175167841E-08, 314.4999014931028682 ) ) ;
#4521 = CARTESIAN_POINT ( 'NONE',  ( -14.84341486352006534, -5.586576249955223616, -439.0021406444614058 ) ) ;
#4522 = LINE ( 'NONE', #447, #865 ) ;
#4523 = ORIENTED_EDGE ( 'NONE', *, *, #6931, .T. ) ;
#4524 = CARTESIAN_POINT ( 'NONE',  ( 14.29183324405000732, 7.414293696095001884, -317.4928077629770087 ) ) ;
#4525 = CARTESIAN_POINT ( 'NONE',  ( -9.065820074235004356, -10.71255845790999572, -317.5770954168139610 ) ) ;
#4526 = CARTESIAN_POINT ( 'NONE',  ( -8.993684809926110191, -9.500000000000001776, -419.2513267189134467 ) ) ;
#4527 = ORIENTED_EDGE ( 'NONE', *, *, #3125, .T. ) ;
#4528 = FACE_OUTER_BOUND ( 'NONE', #5896, .T. ) ;
#4529 = AXIS2_PLACEMENT_3D ( 'NONE', #8639, #4564, #3754 ) ;
#4531 = ORIENTED_EDGE ( 'NONE', *, *, #7731, .F. ) ;
#4530 = VECTOR ( 'NONE', #3470, 1000.000000000000000 ) ;
#4532 = CARTESIAN_POINT ( 'NONE',  ( 14.98664244983999971, -7.043920630080999778, 190.0000000000000000 ) ) ;
#4533 = CARTESIAN_POINT ( 'NONE',  ( -17.04674817168135803, -6.551802883975634373, 319.0000000000003979 ) ) ;
#4534 = ORIENTED_EDGE ( 'NONE', *, *, #6713, .F. ) ;
#4535 = CARTESIAN_POINT ( 'NONE',  ( -11.02833964697000013, -10.42949886550000826, 191.1197171614399792 ) ) ;
#4536 = ORIENTED_EDGE ( 'NONE', *, *, #6814, .T. ) ;
#4537 = CARTESIAN_POINT ( 'NONE',  ( 17.50000000000000711, -8.653813013134384923E-10, -302.5000000000000568 ) ) ;
#4538 = CARTESIAN_POINT ( 'NONE',  ( -18.86301435545000871, 0.4770680115090000228, -302.5071922382879279 ) ) ;
#4539 = CARTESIAN_POINT ( 'NONE',  ( -16.99996037728000076, 1.352916535802999941E-09, -314.9999801883000146 ) ) ;
#4540 = VERTEX_POINT ( 'NONE', #9114 ) ;
#4541 = VECTOR ( 'NONE', #9014, 1000.000000000000000 ) ;
#4542 = VECTOR ( 'NONE', #6823, 1000.000000000000000 ) ;
#4543 = CARTESIAN_POINT ( 'NONE',  ( -1.771702344376552940, -7.457381197138002626, -434.6812846817269929 ) ) ;
#4544 = FILL_AREA_STYLE_COLOUR ( '', #6096 ) ;
#4545 = CARTESIAN_POINT ( 'NONE',  ( 11.24500836742999610, 9.126642939585995151, -302.5071922382879279 ) ) ;
#4546 = APPLICATION_CONTEXT ( 'automotive_design' ) ;
#4547 = CARTESIAN_POINT ( 'NONE',  ( -18.20466326549998470, -5.184475519960003886, 318.8802828394900644 ) ) ;
#4548 = CARTESIAN_POINT ( 'NONE',  ( 16.77957632114000219, -1.244976636274000015, -315.0848619657999734 ) ) ;
#4549 = CARTESIAN_POINT ( 'NONE',  ( -10.49789511286000021, 7.639556387670999982, 314.8616023057000461 ) ) ;
#4550 = ORIENTED_EDGE ( 'NONE', *, *, #8317, .F. ) ;
#4551 = CARTESIAN_POINT ( 'NONE',  ( -26.31853765676889267, -9.500000000000001776, -432.7407288192795249 ) ) ;
#4552 = VERTEX_POINT ( 'NONE', #1747 ) ;
#4553 = CARTESIAN_POINT ( 'NONE',  ( -9.912528015309003848, 10.85837313990000474, 318.8802828394900644 ) ) ;
#4554 = DIRECTION ( 'NONE',  ( -0.9942380540931650135, 0.000000000000000000, -0.1071946444232960011 ) ) ;
#4555 = STYLED_ITEM ( 'NONE', ( #8676 ), #9043 ) ;
#4556 = ORIENTED_EDGE ( 'NONE', *, *, #437, .T. ) ;
#4557 = CARTESIAN_POINT ( 'NONE',  ( -2.000000000000000000, 2.500000000000000000, -404.4999999999999432 ) ) ;
#4558 = CARTESIAN_POINT ( 'NONE',  ( 16.99965680672947954, -0.4176726732850533641, 314.9999999999998863 ) ) ;
#4559 = CARTESIAN_POINT ( 'NONE',  ( -13.95695539824072640, 5.398716172439862682, 315.0000000000000568 ) ) ;
#4560 = CARTESIAN_POINT ( 'NONE',  ( 6.052780067456072999, -5.500000000000000000, -524.2189112390747141 ) ) ;
#4561 = CARTESIAN_POINT ( 'NONE',  ( 14.99960151356000004, 7.033824075090999273, 320.0000000000000000 ) ) ;
#4562 = CARTESIAN_POINT ( 'NONE',  ( -13.92525118639320070, -5.424153755683055245, -314.9999999999999432 ) ) ;
#4563 = CARTESIAN_POINT ( 'NONE',  ( -34.37192209818999800, 2.500000000000000000, -461.0868123482000556 ) ) ;
#4564 = DIRECTION ( 'NONE',  ( 0.000000000000000000, -1.000000000000000000, 0.000000000000000000 ) ) ;
#4565 = CARTESIAN_POINT ( 'NONE',  ( -3.694242493244381365, -7.381371554898000120, -436.9731892404009272 ) ) ;
#4566 = EDGE_CURVE ( 'NONE', #10567, #269, #4919, .T. ) ;
#4567 = CARTESIAN_POINT ( 'NONE',  ( 3.309734165293447550, 9.320883339027414394, -315.0000000000000568 ) ) ;
#4568 = CARTESIAN_POINT ( 'NONE',  ( -16.06649953495000105, 6.900914778667005756, 189.9229057364800042 ) ) ;
#4569 = DIRECTION ( 'NONE',  ( 1.000000000000000000, 0.000000000000000000, 0.000000000000000000 ) ) ;
#4570 = EDGE_CURVE ( 'NONE', #10444, #7389, #8145, .T. ) ;
#4571 = VERTEX_POINT ( 'NONE', #6530 ) ;
#4572 = DIRECTION ( 'NONE',  ( 0.000000000000000000, -1.000000000000000000, 0.000000000000000000 ) ) ;
#4573 = AXIS2_PLACEMENT_3D ( 'NONE', #2803, #1078, #9412 ) ;
#4574 = CARTESIAN_POINT ( 'NONE',  ( -1.736715403303641825, -7.364240132115527082, -434.8724123522787863 ) ) ;
#4575 = CARTESIAN_POINT ( 'NONE',  ( 16.80170962578117155, -1.436180489853609688, 315.0000000000000568 ) ) ;
#4576 = CARTESIAN_POINT ( 'NONE',  ( -13.62823431091000081, 6.408810695481999886, -314.4150829855000211 ) ) ;
#4577 = EDGE_CURVE ( 'NONE', #2473, #8913, #4780, .T. ) ;
#4578 = CARTESIAN_POINT ( 'NONE',  ( -1.604641474886230768, -9.999988122786408695, 314.4999449211996989 ) ) ;
#4579 = CARTESIAN_POINT ( 'NONE',  ( 8.948397653779995409, 10.74758637870000477, 320.0770942683900557 ) ) ;
#4580 = CARTESIAN_POINT ( 'NONE',  ( -0.5093080192647669868, -2.510898790358998767, -434.0830817482614634 ) ) ;
#4581 = ORIENTED_EDGE ( 'NONE', *, *, #7985, .F. ) ;
#4582 = CARTESIAN_POINT ( 'NONE',  ( 1.581094244357999612, 12.05691037822999867, -317.5770954168139610 ) ) ;
#4583 = CARTESIAN_POINT ( 'NONE',  ( 11.79032227421999757, -10.19419839316000065, -317.0792622552969533 ) ) ;
#4584 = PRODUCT_DEFINITION_SHAPE ( 'NONE', 'NONE',  #2387 ) ;
#4585 = DIRECTION ( 'NONE',  ( 0.4716280258120412183, 0.000000000000000000, -0.8817975988108815999 ) ) ;
#4586 = AXIS2_PLACEMENT_3D ( 'NONE', #8881, #4752, #8829 ) ;
#4587 = DIRECTION ( 'NONE',  ( -0.2381566831044910626, 0.000000000000000000, 0.9712267471052612455 ) ) ;
#4588 = VERTEX_POINT ( 'NONE', #5614 ) ;
#4589 = CARTESIAN_POINT ( 'NONE',  ( -16.27944536538999998, 5.903984566639000064, 190.0000000000000000 ) ) ;
#4590 = DIRECTION ( 'NONE',  ( 0.4712473909295827323, 0.000000000000000000, -0.8820010751365675583 ) ) ;
#4591 = EDGE_CURVE ( 'NONE', #7650, #9067, #1799, .T. ) ;
#4592 = VERTEX_POINT ( 'NONE', #10503 ) ;
#4593 = CARTESIAN_POINT ( 'NONE',  ( 12.15874467096999645, -9.926591843472005294, 191.1197171614399792 ) ) ;
#4594 = ORIENTED_EDGE ( 'NONE', *, *, #9414, .T. ) ;
#4595 = DIRECTION ( 'NONE',  ( 0.000000000000000000, -1.000000000000000000, 0.000000000000000000 ) ) ;
#4596 = CARTESIAN_POINT ( 'NONE',  ( 16.59121592455001348, -6.423372090527998068, -302.4229045757450081 ) ) ;
#4597 = CARTESIAN_POINT ( 'NONE',  ( -0.2297665181432845261, -12.00000000000000000, -361.1356115430466502 ) ) ;
#4598 = AXIS2_PLACEMENT_3D ( 'NONE', #2999, #10358, #8578 ) ;
#4599 = CARTESIAN_POINT ( 'NONE',  ( -0.7199992077389804068, -7.501816435716998299, -434.1488804783251112 ) ) ;
#4600 = B_SPLINE_CURVE_WITH_KNOTS ( 'NONE', 3,
 ( #4511, #5364, #8752, #7789 ),
 .UNSPECIFIED., .F., .F.,
 ( 4, 4 ),
 ( 0.000000000000000000, 1.000000000000000000 ),
 .UNSPECIFIED. ) ;
#4601 = CARTESIAN_POINT ( 'NONE',  ( -18.86312040460998674, -0.4763280864498002920, -302.5071922382879279 ) ) ;
#4602 = CARTESIAN_POINT ( 'NONE',  ( 11.00353245304999739, -10.53087951318999593, 319.5792614743400009 ) ) ;
#4603 = LINE ( 'NONE', #3741, #4542 ) ;
#4604 = CARTESIAN_POINT ( 'NONE',  ( -16.21525914616999842, 2.693567875512000054, 315.0848619657999734 ) ) ;
#4605 = VERTEX_POINT ( 'NONE', #1534 ) ;
#4606 = LINE ( 'NONE', #7825, #8594 ) ;
#4607 = CARTESIAN_POINT ( 'NONE',  ( -0.6665706852018948858, -7.499053979551672633, -434.1811903110214530 ) ) ;
#4608 = CYLINDRICAL_SURFACE ( 'NONE', #12, 4.000000000000009770 ) ;
#4609 = CARTESIAN_POINT ( 'NONE',  ( -10.00000000000000000, -2.500000000000000000, -317.5000000000000000 ) ) ;
#4610 = DIRECTION ( 'NONE',  ( 0.000000000000000000, -1.000000000000000000, -0.000000000000000000 ) ) ;
#4611 = CARTESIAN_POINT ( 'NONE',  ( -15.43580712988967107, 3.955371400427518669, 315.0000000000000568 ) ) ;
#4612 = CARTESIAN_POINT ( 'NONE',  ( -17.49999996772987743, -5.857864456328762515, 314.9999999999999432 ) ) ;
#4613 = CARTESIAN_POINT ( 'NONE',  ( -7.529234060647197246, -8.513083068079142279, -315.0000000000000000 ) ) ;
#4614 = CARTESIAN_POINT ( 'NONE',  ( -12.86189865087530038, -4.241237746457299451, -438.9337381460082952 ) ) ;
#4615 =( LENGTH_UNIT ( ) NAMED_UNIT ( * ) SI_UNIT ( .MILLI., .METRE. ) );
#4616 = CARTESIAN_POINT ( 'NONE',  ( -3.713614856666575144E-09, 12.50000000000000000, -316.5000000000000000 ) ) ;
#4617 = VECTOR ( 'NONE', #2192, 1000.000000000000000 ) ;
#4618 = VECTOR ( 'NONE', #8490, 1000.000000000000000 ) ;
#4619 = CARTESIAN_POINT ( 'NONE',  ( 8.647412455283767230, 8.167526177888579042, -315.0000000000000000 ) ) ;
#4620 = ADVANCED_FACE ( 'NONE', ( #6641 ), #4817, .F. ) ;
#4621 = CARTESIAN_POINT ( 'NONE',  ( 19.59059457349998823, 0.06993619660358003920, 189.9229057364800042 ) ) ;
#4622 = CARTESIAN_POINT ( 'NONE',  ( 17.22664556582829931, 1.821222547514791623, 314.4999497328577718 ) ) ;
#4623 = CARTESIAN_POINT ( 'NONE',  ( 18.87000901094000227, -1.611639242563999819, -317.5000000000470095 ) ) ;
#4624 = VECTOR ( 'NONE', #8310, 1000.000000000000000 ) ;
#4625 = EDGE_CURVE ( 'NONE', #9547, #2605, #8485, .T. ) ;
#4626 = DIRECTION ( 'NONE',  ( 0.000000000000000000, 1.000000000000000000, 0.000000000000000000 ) ) ;
#4627 = APPLICATION_PROTOCOL_DEFINITION ( 'draft international standard', 'automotive_design', 1998, #3795 ) ;
#4628 = CARTESIAN_POINT ( 'NONE',  ( 11.33727843270404634, -7.061073773682574384, 315.0000000000000000 ) ) ;
#4629 = ORIENTED_EDGE ( 'NONE', *, *, #8880, .T. ) ;
#4630 = CARTESIAN_POINT ( 'NONE',  ( 10.32396869588999877, 7.471487098147999717, -315.0848619657999734 ) ) ;
#4631 = DIRECTION ( 'NONE',  ( 0.000000000000000000, 1.000000000000000000, 0.000000000000000000 ) ) ;
#4632 = CARTESIAN_POINT ( 'NONE',  ( 16.10430118153999857, 6.867346955731005842, 320.0770942683900557 ) ) ;
#4633 = CARTESIAN_POINT ( 'NONE',  ( -14.74684780783305449, -5.500000000000000000, -439.3959507452315165 ) ) ;
#4634 = CARTESIAN_POINT ( 'NONE',  ( -0.3527150178319009566, -2.477951988898999147, -434.3594990470874109 ) ) ;
#4635 = VERTEX_POINT ( 'NONE', #3253 ) ;
#4636 = CARTESIAN_POINT ( 'NONE',  ( -9.242264416715993747, 10.65406548831999878, -317.5770954168139610 ) ) ;
#4637 = AXIS2_PLACEMENT_3D ( 'NONE', #7576, #7630, #5849 ) ;
#4638 = CARTESIAN_POINT ( 'NONE',  ( -15.92039057294001125, -7.578271297757998681, -316.3802825947000201 ) ) ;
#4639 = CARTESIAN_POINT ( 'NONE',  ( 15.67978886374999803, -4.575336738469999887, -315.0000000000000000 ) ) ;
#4640 = EDGE_CURVE ( 'NONE', #4096, #890, #3147, .T. ) ;
#4641 = CARTESIAN_POINT ( 'NONE',  ( -65.68309414322000350, -2.500000000000000000, -406.3111078829000462 ) ) ;
#4642 = ORIENTED_EDGE ( 'NONE', *, *, #3168, .T. ) ;
#4643 = AXIS2_PLACEMENT_3D ( 'NONE', #8656, #8764, #5485 ) ;
#4644 = CARTESIAN_POINT ( 'NONE',  ( -18.95640219669000004, 0.9217981998336000071, 190.0000000000000000 ) ) ;
#4645 = CARTESIAN_POINT ( 'NONE',  ( 16.99398431597747461, -6.605820200493085714, 319.0000000000003979 ) ) ;
#4646 = ORIENTED_EDGE ( 'NONE', *, *, #5584, .F. ) ;
#4647 = CARTESIAN_POINT ( 'NONE',  ( -1002.398135702230206, -2.500000000000000000, -618.0215964952759577 ) ) ;
#4648 = ORIENTED_EDGE ( 'NONE', *, *, #9438, .F. ) ;
#4649 = CARTESIAN_POINT ( 'NONE',  ( -13.12098914876195366, -6.031629431400056696, 314.9999999999999432 ) ) ;
#4650 = CARTESIAN_POINT ( 'NONE',  ( -19.37583693248997108, -3.422417436021003123, -302.9207377450070453 ) ) ;
#4651 = DIRECTION ( 'NONE',  ( -0.9921831154218024862, 0.000000000000000000, -0.1247904863035890766 ) ) ;
#4652 = CARTESIAN_POINT ( 'NONE',  ( -0.6650832026107983408, -7.510081290281999777, -434.8654298613620881 ) ) ;
#4653 = CIRCLE ( 'NONE', #25, 4.000000000000008882 ) ;
#4654 = SHAPE_REPRESENTATION_RELATIONSHIP ( 'NONE' , 'NONE' ,  #5180, #9043 ) ;
#4655 = CARTESIAN_POINT ( 'NONE',  ( 15.97017057534000450, 7.646575558462997080, -302.9207377450070453 ) ) ;
#4656 = CARTESIAN_POINT ( 'NONE',  ( -0.3140675329811673522, -12.00000000000000000, -361.6501536237392429 ) ) ;
#4657 = ADVANCED_BREP_SHAPE_REPRESENTATION ( '', ( #8917, #2817 ), #5369 ) ;
#4658 = ORIENTED_EDGE ( 'NONE', *, *, #7591, .T. ) ;
#4659 = CARTESIAN_POINT ( 'NONE',  ( -10.58801790939999954, -8.088125079530000150, -314.4150829855000211 ) ) ;
#4660 = CARTESIAN_POINT ( 'NONE',  ( 18.32212638522000248, 3.124911926288000075, -302.5000000000129603 ) ) ;
#4661 = ORIENTED_EDGE ( 'NONE', *, *, #2002, .F. ) ;
#4662 = CARTESIAN_POINT ( 'NONE',  ( 17.84297720825001221, -4.977647671642006166, 189.9229057364800042 ) ) ;
#4663 = CARTESIAN_POINT ( 'NONE',  ( -1.424683970611967609, -7.451261721857263431, -434.6013510996728542 ) ) ;
#4664 = CARTESIAN_POINT ( 'NONE',  ( -14.98500449093754483, -3.491150269972000064, -438.4247239981262396 ) ) ;
#4665 = ORIENTED_EDGE ( 'NONE', *, *, #1694, .F. ) ;
#4666 = CIRCLE ( 'NONE', #1060, 15.50000000000000711 ) ;
#4667 = CARTESIAN_POINT ( 'NONE',  ( 4.001463906138999604, -9.408458373209999337, 314.8616023057000461 ) ) ;
#4668 = CARTESIAN_POINT ( 'NONE',  ( 17.59656075795390606, 5.807225057570236437, 315.0000000000000000 ) ) ;
#4669 = CARTESIAN_POINT ( 'NONE',  ( -15.06605725946605112, 4.378913172242680396, 314.9999999999999432 ) ) ;
#4670 = CARTESIAN_POINT ( 'NONE',  ( -14.24138406224000342, -7.443131114976996976, 319.9928079742500131 ) ) ;
#4671 = CARTESIAN_POINT ( 'NONE',  ( -11.33749276371199066, -7.060967193034008993, -315.0000000000000568 ) ) ;
#4672 = DIRECTION ( 'NONE',  ( 0.9848077530122130163, 0.000000000000000000, 0.1736481776669023813 ) ) ;
#4673 = CARTESIAN_POINT ( 'NONE',  ( -13.22841485905253833, -6.750000122098000155, -437.9939945094035920 ) ) ;
#4674 = VERTEX_POINT ( 'NONE', #7289 ) ;
#4675 = DIRECTION ( 'NONE',  ( -1.000000000000000000, 0.000000000000000000, 0.000000000000000000 ) ) ;
#4676 = CARTESIAN_POINT ( 'NONE',  ( -4.934865307815709201, 9.087242801873953724, -315.0000000000000568 ) ) ;
#4677 = PRODUCT ( 'MAS-686', 'MAS-686', '', ( #1345 ) ) ;
#4678 = CARTESIAN_POINT ( 'NONE',  ( -18.32859070493001852, 4.258570244206002720, 189.9229057364800042 ) ) ;
#4679 = DIRECTION ( 'NONE',  ( 0.000000000000000000, -1.000000000000000000, 0.000000000000000000 ) ) ;
#4680 = CARTESIAN_POINT ( 'NONE',  ( -16.13706688435999581, -6.055114415286000806, -317.5000000000000000 ) ) ;
#4681 = ADVANCED_FACE ( 'NONE', ( #2450 ), #5719, .F. ) ;
#4682 = FACE_OUTER_BOUND ( 'NONE', #5941, .T. ) ;
#4683 = APPLICATION_PROTOCOL_DEFINITION ( 'draft international standard', 'automotive_design', 1998, #5238 ) ;
#4684 = CARTESIAN_POINT ( 'NONE',  ( -12.98706127646999953, 6.788989183774999603, -315.0000000000000000 ) ) ;
#4685 = CARTESIAN_POINT ( 'NONE',  ( 1.257430124576000008, 9.427442400486999219, -315.0848619657999734 ) ) ;
#4686 = PLANE ( 'NONE',  #9440 ) ;
#4687 = VECTOR ( 'NONE', #9382, 1000.000000000000114 ) ;
#4688 = CARTESIAN_POINT ( 'NONE',  ( 20.06710154196001739, -0.4210530330733002757, 319.5792614743400009 ) ) ;
#4689 = CARTESIAN_POINT ( 'NONE',  ( -0.7524131241348165355, -2.498180379936999262, -434.1989882261000275 ) ) ;
#4690 = EDGE_LOOP ( 'NONE', ( #1088, #3080, #5335, #4500 ) ) ;
#4691 = CARTESIAN_POINT ( 'NONE',  ( -12.90264537120001798, 9.651629027462002242, -317.0792622552969533 ) ) ;
#4692 =( BOUNDED_CURVE ( )  B_SPLINE_CURVE ( 3, ( #1931, #4299, #4351, #8476, #9888, #3494, #10047, #4137, #7466, #2690, #5202, #6608, #7624, #1878, #270, #55, #2738, #161, #6827, #109, #5897, #3328, #959, #2525, #5790, #6663, #5844, #10098, #2577, #9135, #1771, #5042, #8324, #4245, #6715, #5093, #7880, #10145, #4449, #6878, #1323, #10202, #2890, #9498, #2994, #3696, #2788, #2137 ),
 .UNSPECIFIED., .F., .F. ) 
 B_SPLINE_CURVE_WITH_KNOTS ( ( 4, 1, 1, 1, 1, 1, 1, 1, 1, 1, 1, 1, 1, 1, 1, 1, 1, 1, 1, 1, 1, 1, 1, 1, 1, 1, 1, 1, 1, 1, 1, 1, 1, 1, 1, 1, 1, 1, 1, 1, 1, 1, 1, 1, 1, 4 ),
 ( 0.000000000000000000, 0.01773478386796093625, 0.03606240600880961100, 0.05363178075044110205, 0.07078725724691559140, 0.08782600590454361922, 0.1049244321358663995, 0.1219539535917413542, 0.1389477140559601531, 0.1563980977818870410, 0.1746363666666245484, 0.1934786392176567060, 0.2128025958997298850, 0.2327904454208187812, 0.2535195744865274547, 0.2747166135707201362, 0.2963888843556201080, 0.3192629785013859078, 0.3441555232881252091, 0.3718650194528618225, 0.4028399612510209504, 0.4371448801346000668, 0.4747436484650962574, 0.5142463203427470875, 0.5531490499891791313, 0.5894092591003683435, 0.6223615841373315583, 0.6515869223714276792, 0.6772431252474833130, 0.7004011076753005050, 0.7222184512862198646, 0.7437909259358920222, 0.7652154438741737286, 0.7858628007620039879, 0.8056883297028475388, 0.8249734464625108066, 0.8436696960199348005, 0.8615821821759909183, 0.8789123401951898229, 0.8960241576542987696, 0.9130500659135333263, 0.9300436868743009455, 0.9471989324631484575, 0.9647777872405111088, 0.9830893744542027468, 1.000000000000000000 ),
 .UNSPECIFIED. ) 
 CURVE ( )  GEOMETRIC_REPRESENTATION_ITEM ( )  RATIONAL_B_SPLINE_CURVE ( ( 1.171573003563706195, 1.171573003563706195, 1.171573003563706195, 1.171573003563706195, 1.171573003563706195, 1.171573003563706195, 1.171573003563706195, 1.171573003563706195, 1.171573003563706195, 1.171573003563706195, 1.171573003563706195, 1.171573003563706195, 1.171573003563706195, 1.171573003563706195, 1.171573003563706195, 1.171573003563706195, 1.171573003563706195, 1.171573003563706195, 1.171573003563706195, 1.171573003563706195, 1.171573003563706195, 1.171573003563706195, 1.171573003563706195, 1.171573003563706195, 1.171573003563706195, 1.171573003563706195, 1.171573003563706195, 1.171573003563706195, 1.171573003563706195, 1.171573003563706195, 1.171573003563706195, 1.171573003563706195, 1.171573003563706195, 1.171573003563706195, 1.171573003563706195, 1.171573003563706195, 1.171573003563706195, 1.171573003563706195, 1.171573003563706195, 1.171573003563706195, 1.171573003563706195, 1.171573003563706195, 1.171573003563706195, 1.171573003563706195, 1.171573003563706195, 1.171573003563706195, 1.171573003563706195, 1.171573003563706195 ) ) 
 REPRESENTATION_ITEM ( '' )  );
#4693 = CARTESIAN_POINT ( 'NONE',  ( -1.601785992426999705, -12.47016740323998718, -316.3802825947000201 ) ) ;
#4694 = ADVANCED_FACE ( 'NONE', ( #9005 ), #6691, .T. ) ;
#4695 = APPLICATION_CONTEXT ( 'automotive_design' ) ;
#4696 = FACE_BOUND ( 'NONE', #9134, .T. ) ;
#4697 = CARTESIAN_POINT ( 'NONE',  ( -46.74071243419621169, -7.500000000000000888, -414.3237589990241077 ) ) ;
#4698 = ORIENTED_EDGE ( 'NONE', *, *, #8571, .F. ) ;
#4699 = CARTESIAN_POINT ( 'NONE',  ( -13.84663869404836412, -6.024484023773889696, -314.5809261257323897 ) ) ;
#4700 = VECTOR ( 'NONE', #2563, 1000.000000000000000 ) ;
#4701 = ORIENTED_EDGE ( 'NONE', *, *, #7615, .T. ) ;
#4702 = CARTESIAN_POINT ( 'NONE',  ( -1.873948611767810357, -7.500000000000000000, -349.2478646809746579 ) ) ;
#4703 = EDGE_LOOP ( 'NONE', ( #1814, #2615, #4556, #8796, #1561, #10304, #3914, #1140, #8214, #1481, #3950, #8480, #10031, #5978, #3245 ) ) ;
#4704 = CARTESIAN_POINT ( 'NONE',  ( -15.60753896450557221, -3.741771784933492828, 315.0000000000000568 ) ) ;
#4705 = CARTESIAN_POINT ( 'NONE',  ( -20.05662131630997536, 0.5622531596958006972, -302.9207377450070453 ) ) ;
#4706 = ADVANCED_FACE ( 'NONE', ( #1857 ), #1910, .T. ) ;
#4707 = CIRCLE ( 'NONE', #2061, 4.000000000000008882 ) ;
#4708 = PLANE ( 'NONE',  #6613 ) ;
#4709 = AXIS2_PLACEMENT_3D ( 'NONE', #1190, #5977, #8447 ) ;
#4710 = AXIS2_PLACEMENT_3D ( 'NONE', #3122, #5696, #9734 ) ;
#4711 =( LENGTH_UNIT ( ) NAMED_UNIT ( * ) SI_UNIT ( .MILLI., .METRE. ) );
#4712 = VECTOR ( 'NONE', #2899, 1000.000000000000000 ) ;
#4713 = CARTESIAN_POINT ( 'NONE',  ( 14.97282077145999679, 8.399840787735001868, -302.9207377450070453 ) ) ;
#4714 = DIRECTION ( 'NONE',  ( 0.9958031466069998672, 0.000000000000000000, 0.09152099872487109988 ) ) ;
#4715 = ORIENTED_EDGE ( 'NONE', *, *, #4277, .F. ) ;
#4716 = CARTESIAN_POINT ( 'NONE',  ( -15.07109120124999890, -4.275483045295999318, -315.0848619657999734 ) ) ;
#4717 = EDGE_CURVE ( 'NONE', #78, #2925, #81, .T. ) ;
#4718 = DIRECTION ( 'NONE',  ( -0.02133028834981354205, 0.000000000000000000, -0.9997724835175820779 ) ) ;
#4719 = ORIENTED_EDGE ( 'NONE', *, *, #9961, .F. ) ;
#4720 = CARTESIAN_POINT ( 'NONE',  ( -4.407678726681998782, -11.78447947993998390, 189.9229057364800042 ) ) ;
#4721 = CARTESIAN_POINT ( 'NONE',  ( -19.99997381626591064, 0.3203551279404593388, 190.9999999999996589 ) ) ;
#4722 = DIRECTION ( 'NONE',  ( 0.9712267471052612455, 7.261373026582001794E-09, 0.2381566831044910626 ) ) ;
#4723 = AXIS2_PLACEMENT_3D ( 'NONE', #5674, #5624, #1652 ) ;
#4724 = AXIS2_PLACEMENT_3D ( 'NONE', #5292, #359, #2881 ) ;
#4725 = ORIENTED_EDGE ( 'NONE', *, *, #2683, .F. ) ;
#4726 = CARTESIAN_POINT ( 'NONE',  ( -16.95904175860000151, -2.156867278632000229, 314.6383426456000052 ) ) ;
#4727 = LINE ( 'NONE', #2145, #2291 ) ;
#4728 = CARTESIAN_POINT ( 'NONE',  ( 13.47907531561000027, 8.083075672345000129, 320.0000000000000000 ) ) ;
#4729 = CARTESIAN_POINT ( 'NONE',  ( -17.75416867407000154, -3.856294574926997232, 319.9928079742500131 ) ) ;
#4730 = DIRECTION ( 'NONE',  ( 0.000000000000000000, 1.000000000000000000, -0.000000000000000000 ) ) ;
#4731 = PLANE ( 'NONE',  #767 ) ;
#4732 = ORIENTED_EDGE ( 'NONE', *, *, #5951, .T. ) ;
#4733 = DIRECTION ( 'NONE',  ( 0.000000000000000000, -1.000000000000000000, 0.000000000000000000 ) ) ;
#4734 =( GEOMETRIC_REPRESENTATION_CONTEXT ( 3 ) GLOBAL_UNCERTAINTY_ASSIGNED_CONTEXT ( ( #5168 ) ) GLOBAL_UNIT_ASSIGNED_CONTEXT ( ( #9021, #9074, #9772 ) ) REPRESENTATION_CONTEXT ( 'NONE', 'WORKASPACE' ) );
#4735 = EDGE_CURVE ( 'NONE', #8275, #4424, #602, .T. ) ;
#4736 = CARTESIAN_POINT ( 'NONE',  ( -14.59598702685000760, 8.048254220853003460, 189.9229057364800042 ) ) ;
#4737 = CARTESIAN_POINT ( 'NONE',  ( 14.91230751981324154, 5.270530829718880206, 314.4999479601416965 ) ) ;
#4738 = CARTESIAN_POINT ( 'NONE',  ( 20.00000000000000000, 4.642020101641720348E-09, -303.5000000000000000 ) ) ;
#4739 =( GEOMETRIC_REPRESENTATION_CONTEXT ( 3 ) GLOBAL_UNCERTAINTY_ASSIGNED_CONTEXT ( ( #4753 ) ) GLOBAL_UNIT_ASSIGNED_CONTEXT ( ( #7848, #4222, #195 ) ) REPRESENTATION_CONTEXT ( 'NONE', 'WORKASPACE' ) );
#4740 = CARTESIAN_POINT ( 'NONE',  ( 15.48936016237493973, 3.890032586757016908, 315.0000000000000000 ) ) ;
#4741 = SHAPE_DEFINITION_REPRESENTATION ( #295, #1739 ) ;
#4742 = CARTESIAN_POINT ( 'NONE',  ( -0.1638132020714603843, -12.51773231663031538, -303.4999999999996589 ) ) ;
#4743 = DIRECTION ( 'NONE',  ( 0.1071946444232947937, 0.000000000000000000, -0.9942380540931651245 ) ) ;
#4744 = DIRECTION ( 'NONE',  ( 0.000000000000000000, 1.000000000000000000, 0.000000000000000000 ) ) ;
#4745 = CARTESIAN_POINT ( 'NONE',  ( -18.69275906597000869, 1.650694058049998469, 319.9928079742500131 ) ) ;
#4746 = DIRECTION ( 'NONE',  ( -0.7784864941891239676, 0.000000000000000000, -0.6276613564376312127 ) ) ;
#4747 = CARTESIAN_POINT ( 'NONE',  ( -1.202539123581771952, -2.515137068876000637, -434.4460766357661328 ) ) ;
#4748 = EDGE_LOOP ( 'NONE', ( #3629, #9256, #1292, #8710 ) ) ;
#4749 = CARTESIAN_POINT ( 'NONE',  ( -9.398723296112997616, 11.12690316796998324, -317.0792622552969533 ) ) ;
#4750 = CARTESIAN_POINT ( 'NONE',  ( 19.31691132429000390, -3.346581979927999217, -316.3802825947000201 ) ) ;
#4751 = EDGE_LOOP ( 'NONE', ( #1913, #2549 ) ) ;
#4752 = DIRECTION ( 'NONE',  ( 0.000000000000000000, -1.000000000000000000, 0.000000000000000000 ) ) ;
#4753 = UNCERTAINTY_MEASURE_WITH_UNIT (LENGTH_MEASURE( 1.000000000000000082E-05 ), #7848, 'distance_accuracy_value', 'NONE');
#4754 = CARTESIAN_POINT ( 'NONE',  ( -0.5579452940971934005, -2.500000333914000006, -434.2759667279211158 ) ) ;
#4755 = FACE_OUTER_BOUND ( 'NONE', #9249, .T. ) ;
#4756 = EDGE_LOOP ( 'NONE', ( #10079, #6301 ) ) ;
#4757 = CARTESIAN_POINT ( 'NONE',  ( -7.848637230397551789, -11.50843006260753931, 319.0000000000003979 ) ) ;
#4758 = ORIENTED_EDGE ( 'NONE', *, *, #2896, .F. ) ;
#4759 = CARTESIAN_POINT ( 'NONE',  ( 18.54292857607040546, 4.743390938996658868, -316.5000000000004547 ) ) ;
#4760 = ORIENTED_EDGE ( 'NONE', *, *, #9427, .T. ) ;
#4761 = CARTESIAN_POINT ( 'NONE',  ( -8.900624420096743705, -8.081841135676405941, 314.9999999999999432 ) ) ;
#4762 = CARTESIAN_POINT ( 'NONE',  ( -6.596975511883001353, -11.38119116100000028, -302.4229045757450081 ) ) ;
#4763 = DIRECTION ( 'NONE',  ( 0.1071946444232954182, 0.000000000000000000, -0.9942380540931651245 ) ) ;
#4764 = SURFACE_SIDE_STYLE ('',( #6204 ) ) ;
#4765 = CARTESIAN_POINT ( 'NONE',  ( 10.56785312427999735, 10.70734743398999811, -302.9207377450070453 ) ) ;
#4766 = CARTESIAN_POINT ( 'NONE',  ( 11.98520373079999679, -10.00909632395999438, 318.8802828394900644 ) ) ;
#4767 = ORIENTED_EDGE ( 'NONE', *, *, #4115, .T. ) ;
#4768 = CARTESIAN_POINT ( 'NONE',  ( 4.001463906138999604, -9.408458373209999337, -314.8616023057000461 ) ) ;
#4769 = CARTESIAN_POINT ( 'NONE',  ( -13.22841524816015202, -3.249999927714000147, -437.9939944912570127 ) ) ;
#4770 = ORIENTED_EDGE ( 'NONE', *, *, #9491, .F. ) ;
#4771 = CARTESIAN_POINT ( 'NONE',  ( -18.85519295008999663, -0.7686777388422003643, 190.0071920248299477 ) ) ;
#4772 = VECTOR ( 'NONE', #8271, 1000.000000000000000 ) ;
#4773 = CARTESIAN_POINT ( 'NONE',  ( 19.79199150660973672, 1.880421430186972387, 190.9999999999996589 ) ) ;
#4774 = FACE_OUTER_BOUND ( 'NONE', #8383, .T. ) ;
#4775 =( BOUNDED_CURVE ( )  B_SPLINE_CURVE ( 3, ( #4039, #7318, #6560, #7263, #8117, #10427, #5531, #8982, #10477, #3119, #4893, #755, #1461, #3067, #6339, #6398, #2320, #4793, #1622, #4742, #10588, #8013, #9677, #5588, #7366, #5, #4843, #3230, #3178, #9842, #8923, #8064, #10534, #6452, #1567, #9788, #9732, #2375, #2426 ),
 .UNSPECIFIED., .F., .T. ) 
 B_SPLINE_CURVE_WITH_KNOTS ( ( 4, 1, 1, 1, 1, 1, 1, 1, 1, 1, 1, 1, 1, 1, 1, 1, 1, 1, 1, 1, 1, 1, 1, 1, 1, 1, 1, 1, 1, 1, 1, 1, 1, 1, 1, 1, 4 ),
 ( 0.000000000000000000, 0.03255837131920313876, 0.06556990764360209889, 0.09473136908033905068, 0.1200161462726948014, 0.1434330934855738704, 0.1672842806195496690, 0.1914679751100890337, 0.2155028411842019875, 0.2393474010340431724, 0.2632466635524260967, 0.2878286224669094340, 0.3134478398786056941, 0.3397600561265991526, 0.3667240395490957150, 0.3951494960372031739, 0.4259522906035831946, 0.4599907034545276940, 0.4966508108602697424, 0.5336723842619189861, 0.5687290606137788140, 0.6006810251919934007, 0.6302097713864017736, 0.6581574700887727891, 0.6853091452815190943, 0.7117521918490830046, 0.7371786555985277989, 0.7617219361653213561, 0.7857512081544899551, 0.8096666007474261351, 0.8337748265625605226, 0.8576111943424252759, 0.8809858201129860955, 0.9062047945899976975, 0.9352885204660792429, 0.9682251798361949380, 1.000000000000000000 ),
 .UNSPECIFIED. ) 
 CURVE ( )  GEOMETRIC_REPRESENTATION_ITEM ( )  RATIONAL_B_SPLINE_CURVE ( ( 1.171573374055207672, 1.171573374055207672, 1.171573374055207895, 1.171573374055207895, 1.171573374055207895, 1.171573374055207895, 1.171573374055207895, 1.171573374055207895, 1.171573374055207895, 1.171573374055207895, 1.171573374055207895, 1.171573374055207895, 1.171573374055207895, 1.171573374055207895, 1.171573374055207895, 1.171573374055207895, 1.171573374055207895, 1.171573374055207895, 1.171573374055207895, 1.171573374055207895, 1.171573374055207895, 1.171573374055207895, 1.171573374055207895, 1.171573374055207895, 1.171573374055207895, 1.171573374055207895, 1.171573374055207895, 1.171573374055207895, 1.171573374055207895, 1.171573374055207895, 1.171573374055207895, 1.171573374055207895, 1.171573374055207895, 1.171573374055207895, 1.171573374055207895, 1.171573374055207895, 1.171573374055207895, 1.171573374055207895, 1.171573374055207895 ) ) 
 REPRESENTATION_ITEM ( '' )  );
#4776 = EDGE_CURVE ( 'NONE', #3582, #8766, #2818, .T. ) ;
#4777 = CARTESIAN_POINT ( 'NONE',  ( -6.419414596134000561, -9.427679607337001499, 314.4150829855000211 ) ) ;
#4778 = SURFACE_STYLE_USAGE ( .BOTH. , #1498 ) ;
#4779 = EDGE_CURVE ( 'NONE', #2605, #9547, #5559, .T. ) ;
#4780 = B_SPLINE_CURVE_WITH_KNOTS ( 'NONE', 3,
 ( #4969, #834, #9867, #9811, #5017, #8196, #8244, #7234, #2347, #4116, #3364, #7444, #3304 ),
 .UNSPECIFIED., .F., .F.,
 ( 4, 1, 1, 1, 1, 1, 1, 1, 1, 1, 4 ),
 ( 0.000000000000000000, 0.08333333333333001192, 0.1666666666667000196, 0.2500000000000000000, 0.3333333333333000081, 0.5000000000000000000, 0.6666666666667000474, 0.7500000000000000000, 0.8333333333333000637, 0.9166666666667000474, 1.000000000000000000 ),
 .UNSPECIFIED. ) ;
#4781 = CARTESIAN_POINT ( 'NONE',  ( -14.17215049938999982, 7.636433089049000422, 320.0000000000000000 ) ) ;
#4782 = CARTESIAN_POINT ( 'NONE',  ( 11.51418862744999139, -9.000691300089004088, 319.9928079742500131 ) ) ;
#4783 = CARTESIAN_POINT ( 'NONE',  ( -19.99999721132999753, 3.518711422920000253E-10, 319.0000000000000000 ) ) ;
#4784 = CARTESIAN_POINT ( 'NONE',  ( -14.84890384377945338, -4.402723804142927300, -438.9797560345791680 ) ) ;
#4785 = FACE_OUTER_BOUND ( 'NONE', #9875, .T. ) ;
#4786 = VERTEX_POINT ( 'NONE', #6854 ) ;
#4787 = DIRECTION ( 'NONE',  ( 1.000000000000000000, 0.000000000000000000, 0.000000000000000000 ) ) ;
#4788 = CARTESIAN_POINT ( 'NONE',  ( -12.90475631688000746, 9.082603241465001531, 189.9229057364800042 ) ) ;
#4789 = FACE_OUTER_BOUND ( 'NONE', #1308, .T. ) ;
#4790 = DIRECTION ( 'NONE',  ( 0.000000000000000000, -1.000000000000000000, 0.000000000000000000 ) ) ;
#4791 = EDGE_CURVE ( 'NONE', #8821, #7857, #4221, .T. ) ;
#4792 = DIRECTION ( 'NONE',  ( 1.000000000000000000, 0.000000000000000000, 0.000000000000000000 ) ) ;
#4793 = CARTESIAN_POINT ( 'NONE',  ( -3.693615097834042516, -12.29963531854552272, -303.4999999999996589 ) ) ;
#4794 = ORIENTED_EDGE ( 'NONE', *, *, #88, .F. ) ;
#4795 = CARTESIAN_POINT ( 'NONE',  ( -16.89041368998000081, -5.257268626091000208, -302.5000000000009663 ) ) ;
#4796 =( LENGTH_UNIT ( ) NAMED_UNIT ( * ) SI_UNIT ( .MILLI., .METRE. ) );
#4797 = CARTESIAN_POINT ( 'NONE',  ( -4.335116381453002710, 11.79481621787999757, 320.0770942683900557 ) ) ;
#4798 = CARTESIAN_POINT ( 'NONE',  ( -1.177149113458909824, -2.596052473566999641, -434.6509312389400748 ) ) ;
#4799 = VERTEX_POINT ( 'NONE', #8404 ) ;
#4800 = CARTESIAN_POINT ( 'NONE',  ( -13.71837527932998491, 8.620941849619004671, -317.5770954168139610 ) ) ;
#4801 = CARTESIAN_POINT ( 'NONE',  ( -2.000000000003786749, -9.000000000000001776, -409.4999999999758415 ) ) ;
#4802 = AXIS2_PLACEMENT_3D ( 'NONE', #5116, #1139, #238 ) ;
#4803 = CYLINDRICAL_SURFACE ( 'NONE', #4586, 3.500000000000003109 ) ;
#4804 = VERTEX_POINT ( 'NONE', #6752 ) ;
#4805 = DIRECTION ( 'NONE',  ( 0.000000000000000000, 1.000000000000000000, 0.000000000000000000 ) ) ;
#4806 = CARTESIAN_POINT ( 'NONE',  ( 16.91992689674542660, -1.077645906677548338, -315.0000000000000000 ) ) ;
#4807 = ADVANCED_FACE ( 'NONE', ( #936 ), #6062, .F. ) ;
#4808 = ORIENTED_EDGE ( 'NONE', *, *, #9552, .F. ) ;
#4809 = CIRCLE ( 'NONE', #3, 0.5000000000000004441 ) ;
#4810 = CARTESIAN_POINT ( 'NONE',  ( 14.75365836417945431, -8.451130538707891660, 319.0000000000003979 ) ) ;
#4811 = ORIENTED_EDGE ( 'NONE', *, *, #8403, .T. ) ;
#4812 = CARTESIAN_POINT ( 'NONE',  ( -18.99984327789000105, 0.5550485914519999175, -317.4999999998989892 ) ) ;
#4813 = VERTEX_POINT ( 'NONE', #6340 ) ;
#4814 = CARTESIAN_POINT ( 'NONE',  ( -4.648656036509398959, -9.134414902114890822, 315.0000000000000568 ) ) ;
#4815 = CARTESIAN_POINT ( 'NONE',  ( 6.445113046380004818, -11.41524423681998712, -302.4229045757450081 ) ) ;
#4816 = CARTESIAN_POINT ( 'NONE',  ( -13.36185104352900055, -9.000000000000001776, -400.1641368440791098 ) ) ;
#4817 = CYLINDRICAL_SURFACE ( 'NONE', #9183, 4.000000000000009770 ) ;
#4818 = CIRCLE ( 'NONE', #7874, 11.99999999999997691 ) ;
#4819 = ADVANCED_FACE ( 'NONE', ( #3880 ), #9624, .F. ) ;
#4820 = CARTESIAN_POINT ( 'NONE',  ( 20.10115407781998442, 0.3730669878444000664, -302.9207377450070453 ) ) ;
#4821 = CARTESIAN_POINT ( 'NONE',  ( -11.22625503481000209, -10.34655023142000907, 318.8802828394900644 ) ) ;
#4822 = ORIENTED_EDGE ( 'NONE', *, *, #670, .T. ) ;
#4823 = CARTESIAN_POINT ( 'NONE',  ( -15.71297435277999810, -3.490404421959999670, -315.0848619657999734 ) ) ;
#4824 = CARTESIAN_POINT ( 'NONE',  ( -72.90663470096859555, -7.500000000000000000, -371.7168990827444190 ) ) ;
#4825 = ORIENTED_EDGE ( 'NONE', *, *, #5112, .F. ) ;
#4826 = CARTESIAN_POINT ( 'NONE',  ( -9.832070176257998284, -10.44777315889000313, 189.9229057364800042 ) ) ;
#4827 = CARTESIAN_POINT ( 'NONE',  ( 0.7126779659676973910, 12.51265294199208000, 190.9999999999996589 ) ) ;
#4828 = DIRECTION ( 'NONE',  ( -0.8820010751365675583, 0.000000000000000000, -0.4712473909295827323 ) ) ;
#4829 = EDGE_CURVE ( 'NONE', #8632, #9766, #1976, .T. ) ;
#4830 = CARTESIAN_POINT ( 'NONE',  ( -3.903842856253999738, -9.647088721075000706, 314.6383426456000052 ) ) ;
#4831 = CARTESIAN_POINT ( 'NONE',  ( -12.48775874806000097, 8.649334263351001084, 320.0000000000000000 ) ) ;
#4832 = DIRECTION ( 'NONE',  ( 0.000000000000000000, 1.000000000000000000, 0.000000000000000000 ) ) ;
#4833 = CARTESIAN_POINT ( 'NONE',  ( 7.848637230397552678, 11.50843006260754109, 319.0000000000005116 ) ) ;
#4834 = LINE ( 'NONE', #9613, #5906 ) ;
#4835 = ORIENTED_EDGE ( 'NONE', *, *, #833, .T. ) ;
#4836 = CARTESIAN_POINT ( 'NONE',  ( -15.00000000000000000, 0.4945770392355999800, -285.0000000000000000 ) ) ;
#4837 = EDGE_LOOP ( 'NONE', ( #4246, #5068, #2527, #7678 ) ) ;
#4838 = EDGE_CURVE ( 'NONE', #10018, #4161, #7368, .T. ) ;
#4839 = AXIS2_PLACEMENT_3D ( 'NONE', #2367, #4733, #6327 ) ;
#4840 = EDGE_LOOP ( 'NONE', ( #2175, #7200, #9739, #8356 ) ) ;
#4841 = FACE_OUTER_BOUND ( 'NONE', #6864, .T. ) ;
#4842 = CARTESIAN_POINT ( 'NONE',  ( 16.68818136459866253, 1.819152193222137059, 315.0000000000000000 ) ) ;
#4843 = CARTESIAN_POINT ( 'NONE',  ( 10.52063983335276731, -10.64371280159997468, -303.4999999999996589 ) ) ;
#4844 = CARTESIAN_POINT ( 'NONE',  ( 15.07109120124999890, 4.275483045295999318, -315.0848619657999734 ) ) ;
#4845 = CARTESIAN_POINT ( 'NONE',  ( -24.05731444175778577, -7.500000000000000000, -497.1993521173619683 ) ) ;
#4846 = AXIS2_PLACEMENT_3D ( 'NONE', #7229, #10496, #2339 ) ;
#4847 = CARTESIAN_POINT ( 'NONE',  ( -2.291122522771679382, -7.236295659725429985, -435.5124405936905987 ) ) ;
#4848 = CARTESIAN_POINT ( 'NONE',  ( -19.85665319583999988, 1.941121513171000901, 319.5792614743400009 ) ) ;
#4849 = CARTESIAN_POINT ( 'NONE',  ( -14.98500449093754838, -6.362323852810936486, -438.4247239981263533 ) ) ;
#4850 = VECTOR ( 'NONE', #10464, 1000.000000000000000 ) ;
#4851 = CARTESIAN_POINT ( 'NONE',  ( -0.8204922433515965396, -2.522492683188001461, -434.9474946677987077 ) ) ;
#4852 = VERTEX_POINT ( 'NONE', #10428 ) ;
#4853 = CARTESIAN_POINT ( 'NONE',  ( 7.885457619219000236, 11.57957576882999184, -317.0792622552969533 ) ) ;
#4854 = CARTESIAN_POINT ( 'NONE',  ( 16.87780931964001141, -6.722286650069999148, -316.3802825947000201 ) ) ;
#4855 = ORIENTED_EDGE ( 'NONE', *, *, #2474, .T. ) ;
#4856 = CARTESIAN_POINT ( 'NONE',  ( 17.80730577449000052, -3.998365122558999563, 320.0000000000000000 ) ) ;
#4857 = CARTESIAN_POINT ( 'NONE',  ( -0.8115155145918805379, -7.442392689726998967, -434.4760555596726022 ) ) ;
#4858 = VECTOR ( 'NONE', #6300, 1000.000000000000000 ) ;
#4859 = DIRECTION ( 'NONE',  ( -2.134661488198361529E-05, -5.799867325201099395E-11, -0.9999999997721611411 ) ) ;
#4860 = CARTESIAN_POINT ( 'NONE',  ( -6.348506474365286145, 9.305625771097020049, -314.5281326612878843 ) ) ;
#4861 = ORIENTED_EDGE ( 'NONE', *, *, #5217, .T. ) ;
#4862 = CARTESIAN_POINT ( 'NONE',  ( 19.95988936745280640, -0.9706423173584770581, 319.0000000000003979 ) ) ;
#4863 = VERTEX_POINT ( 'NONE', #6508 ) ;
#4864 = CARTESIAN_POINT ( 'NONE',  ( -3.763664787428660841, 12.29131725939111597, -316.5000000000004547 ) ) ;
#4865 = ORIENTED_EDGE ( 'NONE', *, *, #309, .F. ) ;
#4866 = CARTESIAN_POINT ( 'NONE',  ( 19.87644374459000929, -1.701742232560001788, -303.6197174156520759 ) ) ;
#4867 = DIRECTION ( 'NONE',  ( 0.000000000000000000, -1.000000000000000000, 0.000000000000000000 ) ) ;
#4868 = FACE_OUTER_BOUND ( 'NONE', #4436, .T. ) ;
#4869 = CARTESIAN_POINT ( 'NONE',  ( 12.85183647427999176, 9.678193536939003749, -302.9207377450070453 ) ) ;
#4870 = VECTOR ( 'NONE', #3685, 1000.000000000000000 ) ;
#4871 = DIRECTION ( 'NONE',  ( -0.000000000000000000, 1.000000000000000000, 0.000000000000000000 ) ) ;
#4872 = VERTEX_POINT ( 'NONE', #8176 ) ;
#4873 = CARTESIAN_POINT ( 'NONE',  ( -1.285290206351000108, -10.09749793447999977, -314.4150829855000211 ) ) ;
#4874 = CARTESIAN_POINT ( 'NONE',  ( 14.32653628403999946, 7.536184728883000616, -302.5000000000000000 ) ) ;
#4875 = EDGE_LOOP ( 'NONE', ( #2241, #401, #1236 ) ) ;
#4876 = CARTESIAN_POINT ( 'NONE',  ( -6.027267673561996553, -11.50416862954998365, 189.9229057364800042 ) ) ;
#4877 = CARTESIAN_POINT ( 'NONE',  ( -72.90663470102438737, -12.50000000000000000, -368.3168990826883373 ) ) ;
#4878 = CARTESIAN_POINT ( 'NONE',  ( 4.603216684274966219, 9.141664750100051862, -315.0000000000000568 ) ) ;
#4879 = FACE_OUTER_BOUND ( 'NONE', #5632, .T. ) ;
#4880 = CIRCLE ( 'NONE', #5730, 0.5000000000000004441 ) ;
#4881 = CARTESIAN_POINT ( 'NONE',  ( -16.75097866579000083, -2.074182492207000461, 314.8616023057000461 ) ) ;
#4882 =( NAMED_UNIT ( * ) PLANE_ANGLE_UNIT ( ) SI_UNIT ( $, .RADIAN. ) );
#4883 = FACE_OUTER_BOUND ( 'NONE', #7809, .T. ) ;
#4884 = CARTESIAN_POINT ( 'NONE',  ( -18.87181153733000016, 0.3572136203155001355, 319.9928079742500131 ) ) ;
#4885 = CARTESIAN_POINT ( 'NONE',  ( -2.572515036489481766, 12.41549478438273724, 319.0000000000005116 ) ) ;
#4886 = CARTESIAN_POINT ( 'NONE',  ( 14.79012398733999945, 1.483731117707000058, 315.0000000000000000 ) ) ;
#4887 = ORIENTED_EDGE ( 'NONE', *, *, #121, .T. ) ;
#4888 = CARTESIAN_POINT ( 'NONE',  ( -72.90663470102438737, -12.50000000000000000, -375.1168990826883487 ) ) ;
#4889 = AXIS2_PLACEMENT_3D ( 'NONE', #10415, #7253, #8972 ) ;
#4890 = AXIS2_PLACEMENT_3D ( 'NONE', #6152, #463, #7078 ) ;
#4891 = CARTESIAN_POINT ( 'NONE',  ( -15.00000000000000000, 0.000000000000000000, 315.0000000000000000 ) ) ;
#4892 = CARTESIAN_POINT ( 'NONE',  ( 16.40981772118269788, 2.462276419762760682, 314.9999999999999432 ) ) ;
#4893 = CARTESIAN_POINT ( 'NONE',  ( -12.81623431846863603, -9.609762277177447132, -303.4999999999996589 ) ) ;
#4894 = CARTESIAN_POINT ( 'NONE',  ( 17.36972170382999892, 0.04551883977364000466, -314.6383426456000052 ) ) ;
#4895 = EDGE_CURVE ( 'NONE', #8331, #4386, #5394, .T. ) ;
#4896 = DIRECTION ( 'NONE',  ( -0.9921831154218023752, 0.000000000000000000, -0.1247904863035890627 ) ) ;
#4897 = CYLINDRICAL_SURFACE ( 'NONE', #7415, 12.49999999999998757 ) ;
#4898 = DIRECTION ( 'NONE',  ( 0.000000000000000000, -1.000000000000000000, 0.000000000000000000 ) ) ;
#4899 = EDGE_CURVE ( 'NONE', #4067, #4512, #1020, .T. ) ;
#4900 = CARTESIAN_POINT ( 'NONE',  ( -76.74404526914973701, -8.000000000000000000, -359.2961792914830426 ) ) ;
#4901 = CARTESIAN_POINT ( 'NONE',  ( -1.873948611771682149, -12.50000000000000000, -349.2478646809681777 ) ) ;
#4902 = CARTESIAN_POINT ( 'NONE',  ( 3.365463313584999838, 12.41489380075000604, -317.0792622552969533 ) ) ;
#4903 = DIRECTION ( 'NONE',  ( 0.1247904863035870365, 0.000000000000000000, -0.9921831154218027082 ) ) ;
#4904 = PRESENTATION_LAYER_ASSIGNMENT (  '', '', ( #3188 ) ) ;
#4905 = CARTESIAN_POINT ( 'NONE',  ( -8.770005493155000664, -10.19600538561000036, 320.0000000000000000 ) ) ;
#4906 = EDGE_CURVE ( 'NONE', #7180, #6903, #2141, .T. ) ;
#4907 = CARTESIAN_POINT ( 'NONE',  ( -0.3216191152362427585, -7.544227617881000825, -433.9889066583573367 ) ) ;
#4908 = CARTESIAN_POINT ( 'NONE',  ( -19.00000000000000000, 0.000000000000000000, -317.4999999998989892 ) ) ;
#4909 = EDGE_CURVE ( 'NONE', #6716, #3828, #1631, .T. ) ;
#4910 = CARTESIAN_POINT ( 'NONE',  ( 15.45543459605807968, -3.931565522428362325, -315.0000000000000568 ) ) ;
#4911 = ORIENTED_EDGE ( 'NONE', *, *, #9496, .F. ) ;
#4912 = AXIS2_PLACEMENT_3D ( 'NONE', #5127, #2962, #1805 ) ;
#4913 = CARTESIAN_POINT ( 'NONE',  ( 15.67978886374999803, 4.575336738469999887, -314.4963898845653603 ) ) ;
#4914 = EDGE_LOOP ( 'NONE', ( #10318, #2058, #9814, #9399 ) ) ;
#4915 = CARTESIAN_POINT ( 'NONE',  ( 1.614076495133000000, 11.47540331082000087, -317.5000000000000000 ) ) ;
#4916 = ORIENTED_EDGE ( 'NONE', *, *, #2464, .T. ) ;
#4917 = CARTESIAN_POINT ( 'NONE',  ( 16.01368207331000093, -7.610776120867003947, -302.9207377450070453 ) ) ;
#4918 = CARTESIAN_POINT ( 'NONE',  ( -1.873948611767810357, -7.500000000000000000, -349.2478646809746579 ) ) ;
#4919 = LINE ( 'NONE', #3954, #3171 ) ;
#4920 = CARTESIAN_POINT ( 'NONE',  ( 18.53523119387001117, 4.742105934366003694, -303.6197174156509391 ) ) ;
#4921 = EDGE_CURVE ( 'NONE', #5915, #8113, #2581, .T. ) ;
#4922 = CARTESIAN_POINT ( 'NONE',  ( 1.279516016521960085E-07, 10.00000000000000000, 315.0000000000000000 ) ) ;
#4923 = VERTEX_POINT ( 'NONE', #224 ) ;
#4924 = CARTESIAN_POINT ( 'NONE',  ( -16.95904175860000151, -2.156867278632000229, -314.6383426456000052 ) ) ;
#4925 = CYLINDRICAL_SURFACE ( 'NONE', #6959, 3.499999999999999112 ) ;
#4926 = EDGE_LOOP ( 'NONE', ( #3030, #3847, #6589, #3377 ) ) ;
#4927 = CARTESIAN_POINT ( 'NONE',  ( -15.65104815535000071, -7.893060908445997725, 190.4207385301700128 ) ) ;
#4928 = CARTESIAN_POINT ( 'NONE',  ( -19.95972666420564323, 0.9723020053078084146, 190.9999999999996305 ) ) ;
#4929 = CARTESIAN_POINT ( 'NONE',  ( 16.33391464646021873, 2.612996577909529439, -314.9999999999999432 ) ) ;
#4930 = CARTESIAN_POINT ( 'NONE',  ( -17.18550143358999449, -2.500000000000000000, -495.8459145668000474 ) ) ;
#4931 = CARTESIAN_POINT ( 'NONE',  ( 16.89986669904000394, -0.5583209492923999484, 315.0848619657999734 ) ) ;
#4932 = CARTESIAN_POINT ( 'NONE',  ( -46.74071243419621169, -7.500000000000000888, -414.3237589990241077 ) ) ;
#4933 = CARTESIAN_POINT ( 'NONE',  ( -15.40147079910000372, -7.455286574312999903, 320.0770942683900557 ) ) ;
#4934 = VECTOR ( 'NONE', #2144, 1000.000000000000000 ) ;
#4935 = CARTESIAN_POINT ( 'NONE',  ( -18.18176685080253918, 5.227975112149439774, 319.0000000000005116 ) ) ;
#4936 = CARTESIAN_POINT ( 'NONE',  ( 11.70471109486296868, 10.14826236475114740, -303.5000000000000000 ) ) ;
#4937 = DIRECTION ( 'NONE',  ( 0.000000000000000000, -1.000000000000000000, 0.000000000000000000 ) ) ;
#4938 = VERTEX_POINT ( 'NONE', #4997 ) ;
#4939 = CARTESIAN_POINT ( 'NONE',  ( 17.49999999954662044, -9.625715914672042649E-06, 190.0000000000000000 ) ) ;
#4940 = ORIENTED_EDGE ( 'NONE', *, *, #27, .F. ) ;
#4941 = AXIS2_PLACEMENT_3D ( 'NONE', #9341, #2935, #6153 ) ;
#4942 = CARTESIAN_POINT ( 'NONE',  ( -20.00000000000000000, 7.277416212200430041E-10, -316.5000000000000000 ) ) ;
#4943 = CARTESIAN_POINT ( 'NONE',  ( 16.37744599325981909, 2.527607301898085801, 314.9999999999999432 ) ) ;
#4944 = CARTESIAN_POINT ( 'NONE',  ( 15.00000000000000000, -0.4945770392355999800, -285.0000000000000000 ) ) ;
#4945 = CARTESIAN_POINT ( 'NONE',  ( 17.59334121105999671, 0.04733121045982999903, -314.4150829855000211 ) ) ;
#4946 = CARTESIAN_POINT ( 'NONE',  ( -10.00000000000000000, -2.500000000000000000, -272.5000000000000000 ) ) ;
#4947 = EDGE_CURVE ( 'NONE', #8268, #111, #3502, .T. ) ;
#4948 = CARTESIAN_POINT ( 'NONE',  ( -14.98664244983999971, 7.043920630080999778, 190.0000000000000000 ) ) ;
#4949 = CARTESIAN_POINT ( 'NONE',  ( -14.97800895934490484, -6.224293360900853500, -438.4532524748601645 ) ) ;
#4950 = CARTESIAN_POINT ( 'NONE',  ( -19.99999721132999753, 3.518711422920000253E-10, 319.0000000000000000 ) ) ;
#4951 = DIRECTION ( 'NONE',  ( 0.000000000000000000, 1.000000000000000000, 0.000000000000000000 ) ) ;
#4952 = CARTESIAN_POINT ( 'NONE',  ( -14.96823785528000528, 8.299997444912003530, -316.3802825947000201 ) ) ;
#4953 = EDGE_CURVE ( 'NONE', #8445, #2874, #912, .T. ) ;
#4954 = ORIENTED_EDGE ( 'NONE', *, *, #5793, .T. ) ;
#4955 = CARTESIAN_POINT ( 'NONE',  ( 9.597846547914999249, -9.915773017694000657, 320.0000000000000000 ) ) ;
#4956 = EDGE_CURVE ( 'NONE', #9192, #6833, #6670, .T. ) ;
#4957 = CARTESIAN_POINT ( 'NONE',  ( -0.2499204815635852339, -7.611303227785001013, -434.5371318843381232 ) ) ;
#4958 = PRODUCT_DEFINITION_CONTEXT ( 'detailed design', #8451, 'design' ) ;
#4959 = CARTESIAN_POINT ( 'NONE',  ( -76.74404526916885061, -12.00000000000000000, -359.2961792914889543 ) ) ;
#4960 = CARTESIAN_POINT ( 'NONE',  ( 2.737251867098380753, -9.374957062059573687, -315.0000000000000000 ) ) ;
#4961 = VERTEX_POINT ( 'NONE', #536 ) ;
#4962 = CARTESIAN_POINT ( 'NONE',  ( 8.037373804805000077, 9.179324345868998591, -314.4963898845653603 ) ) ;
#4963 = ORIENTED_EDGE ( 'NONE', *, *, #6072, .F. ) ;
#4964 = CARTESIAN_POINT ( 'NONE',  ( -3.698987565691999713, 11.29118203779999874, -317.5000000000000000 ) ) ;
#4965 = ORIENTED_EDGE ( 'NONE', *, *, #1084, .T. ) ;
#4966 = CARTESIAN_POINT ( 'NONE',  ( 20.10149561490999659, -0.3453761138107002138, -302.9207377450070453 ) ) ;
#4967 = AXIS2_PLACEMENT_3D ( 'NONE', #1576, #9687, #3075 ) ;
#4968 = CARTESIAN_POINT ( 'NONE',  ( 5.133129775586001031, -10.95790389472999316, -317.4928077629770087 ) ) ;
#4969 = CARTESIAN_POINT ( 'NONE',  ( -15.00000000000000000, 0.000000000000000000, 315.0000000000000000 ) ) ;
#4970 = VECTOR ( 'NONE', #968, 1000.000000000000000 ) ;
#4971 = CARTESIAN_POINT ( 'NONE',  ( -15.02162735728999543, 8.365494092177003793, -302.9207377450070453 ) ) ;
#4972 = DIRECTION ( 'NONE',  ( -0.9554399839384177806, 0.000000000000000000, -0.2951854283188049544 ) ) ;
#4973 = ORIENTED_EDGE ( 'NONE', *, *, #1113, .T. ) ;
#4974 = DIRECTION ( 'NONE',  ( 0.000000000000000000, -1.000000000000000000, 0.000000000000000000 ) ) ;
#4975 = LINE ( 'NONE', #9231, #4541 ) ;
#4976 = ORIENTED_EDGE ( 'NONE', *, *, #1146, .T. ) ;
#4977 = CARTESIAN_POINT ( 'NONE',  ( -20.06711733022002164, 0.4206966322103999900, 190.4207385301700128 ) ) ;
#4978 = CARTESIAN_POINT ( 'NONE',  ( 17.50000000000125056, 1.380497925828168986E-12, -314.4944826805096341 ) ) ;
#4979 = CARTESIAN_POINT ( 'NONE',  ( 16.78721195431734259, 1.718634075882272239, -314.9999999999999432 ) ) ;
#4980 = CARTESIAN_POINT ( 'NONE',  ( -16.98100918689000238, -2.633704000000000267, -439.4179428962999623 ) ) ;
#4981 = CARTESIAN_POINT ( 'NONE',  ( -13.99304003883001180, 8.933243331610997373, 191.1197171614399792 ) ) ;
#4982 = AXIS2_PLACEMENT_3D ( 'NONE', #3823, #9280, #1047 ) ;
#4983 = LINE ( 'NONE', #103, #9576 ) ;
#4984 =( LENGTH_UNIT ( ) NAMED_UNIT ( * ) SI_UNIT ( .MILLI., .METRE. ) );
#4985 = CARTESIAN_POINT ( 'NONE',  ( -72.90663470102438737, -12.50000000000000000, -371.7168990826883714 ) ) ;
#4986 = CARTESIAN_POINT ( 'NONE',  ( -16.10430118153999857, -6.867346955731005842, 320.0770942683900557 ) ) ;
#4987 = CARTESIAN_POINT ( 'NONE',  ( -72.90663470102438737, -12.50000000000000000, -375.1168990826883487 ) ) ;
#4988 = CARTESIAN_POINT ( 'NONE',  ( 8.450675645183000739, 8.177559542660000957, 315.0848619657999734 ) ) ;
#4989 = VECTOR ( 'NONE', #8099, 1000.000000000000000 ) ;
#4990 = ORIENTED_EDGE ( 'NONE', *, *, #3001, .T. ) ;
#4991 = DIRECTION ( 'NONE',  ( -1.000000000000000000, 0.000000000000000000, 0.000000000000000000 ) ) ;
#4992 = ORIENTED_EDGE ( 'NONE', *, *, #2791, .T. ) ;
#4993 = CARTESIAN_POINT ( 'NONE',  ( -10.02519493912904380, 7.672398658596809362, 315.0000000000000568 ) ) ;
#4994 = DIRECTION ( 'NONE',  ( -6.262351748276267552E-13, -1.000000000000000000, 1.110223024625155531E-12 ) ) ;
#4995 = VECTOR ( 'NONE', #9583, 1000.000000000000000 ) ;
#4996 = ORIENTED_EDGE ( 'NONE', *, *, #422, .T. ) ;
#4997 = CARTESIAN_POINT ( 'NONE',  ( 10.54676984209158519, -7.500000000000000000, -347.8422498368975084 ) ) ;
#4998 = CARTESIAN_POINT ( 'NONE',  ( 18.53584076651999979, 2.541936159385000060, 190.0000000000000000 ) ) ;
#4999 = CARTESIAN_POINT ( 'NONE',  ( -14.98500449093754483, -3.250000000000000444, -438.4247239981262396 ) ) ;
#5000 = FACE_OUTER_BOUND ( 'NONE', #9726, .T. ) ;
#5001 = CARTESIAN_POINT ( 'NONE',  ( -2.055393166047998932, 12.44351316864999824, -316.3802825947000201 ) ) ;
#5002 = EDGE_CURVE ( 'NONE', #6684, #5593, #1326, .T. ) ;
#5003 = DIRECTION ( 'NONE',  ( 0.2951854283188045658, 0.000000000000000000, -0.9554399839384175586 ) ) ;
#5004 = CARTESIAN_POINT ( 'NONE',  ( -0.4024097121659061527, -7.571118624678998543, -434.6905673336279392 ) ) ;
#5005 = AXIS2_PLACEMENT_3D ( 'NONE', #8670, #2877, #8514 ) ;
#5006 = CARTESIAN_POINT ( 'NONE',  ( -85.79375217459825365, -7.500000000000000000, -343.3529193039154279 ) ) ;
#5007 = CARTESIAN_POINT ( 'NONE',  ( 16.40967564559107572, -2.462589562615133065, -315.0000000000000000 ) ) ;
#5008 = ORIENTED_EDGE ( 'NONE', *, *, #7600, .F. ) ;
#5009 = ADVANCED_FACE ( 'NONE', ( #9359 ), #8690, .T. ) ;
#5010 = CARTESIAN_POINT ( 'NONE',  ( 12.98706127646999953, 6.788989183774999603, -315.0000000000001137 ) ) ;
#5011 = ORIENTED_EDGE ( 'NONE', *, *, #5342, .T. ) ;
#5012 = CARTESIAN_POINT ( 'NONE',  ( 11.26076953950000004, 9.251451169536998975, -317.5000000000000000 ) ) ;
#5013 = ORIENTED_EDGE ( 'NONE', *, *, #7529, .F. ) ;
#5014 = CARTESIAN_POINT ( 'NONE',  ( -16.84215363705000712, -6.757103037815999969, -303.6197174156509391 ) ) ;
#5015 = ADVANCED_FACE ( 'NONE', ( #6888 ), #377, .F. ) ;
#5016 = CARTESIAN_POINT ( 'NONE',  ( 13.35621109890998959, -8.022534180767001644, -317.4928077629770087 ) ) ;
#5017 = CARTESIAN_POINT ( 'NONE',  ( -11.28781796570999951, -4.951468039558000633, 315.0000000000000000 ) ) ;
#5018 =( NAMED_UNIT ( * ) SI_UNIT ( $, .STERADIAN. ) SOLID_ANGLE_UNIT ( ) );
#5019 = CARTESIAN_POINT ( 'NONE',  ( -20.05676974677001922, -0.5613724988767001545, -302.9207377450070453 ) ) ;
#5020 = CARTESIAN_POINT ( 'NONE',  ( -64.74703706733102138, -7.500000000000000888, -381.8372235071499290 ) ) ;
#5021 = EDGE_LOOP ( 'NONE', ( #7132, #8006, #202, #3913, #943 ) ) ;
#5022 = FACE_OUTER_BOUND ( 'NONE', #4321, .T. ) ;
#5023 = ADVANCED_FACE ( 'NONE', ( #10363 ), #2900, .T. ) ;
#5024 = CARTESIAN_POINT ( 'NONE',  ( -101.0297452788102817, -2.500000000000000000, -342.4231267849074811 ) ) ;
#5025 = EDGE_LOOP ( 'NONE', ( #750, #2117, #8731, #2917 ) ) ;
#5026 = CARTESIAN_POINT ( 'NONE',  ( -20.04745173227997768, -0.9063373766989004654, 190.4207385301700128 ) ) ;
#5027 = DIRECTION ( 'NONE',  ( 0.000000000000000000, -1.000000000000000000, 0.000000000000000000 ) ) ;
#5028 = DIRECTION ( 'NONE',  ( -0.2951854283188052319, 0.000000000000000000, 0.9554399839384175586 ) ) ;
#5029 = EDGE_CURVE ( 'NONE', #8305, #4804, #7684, .T. ) ;
#5030 = DIRECTION ( 'NONE',  ( -0.000000000000000000, 1.000000000000000000, 0.000000000000000000 ) ) ;
#5031 = CARTESIAN_POINT ( 'NONE',  ( -1.248913580286000302, 12.48838264809999643, 191.1197171614399792 ) ) ;
#5032 = MECHANICAL_DESIGN_GEOMETRIC_PRESENTATION_REPRESENTATION (  '', ( #5209 ), #7957 ) ;
#5033 = CARTESIAN_POINT ( 'NONE',  ( 8.759386130138000937, -8.782224002452998946, 314.4150829855000211 ) ) ;
#5034 = EDGE_CURVE ( 'NONE', #9136, #6684, #312, .T. ) ;
#5035 = DIRECTION ( 'NONE',  ( -0.5828070674935414974, 0.000000000000000000, -0.8126105599114366029 ) ) ;
#5036 = CARTESIAN_POINT ( 'NONE',  ( -11.06499621481999895, -9.965574156584002807, 320.0770942683900557 ) ) ;
#5037 = CARTESIAN_POINT ( 'NONE',  ( -86.49427212956700828, -2.500000000000000000, -350.5299153184531633 ) ) ;
#5038 = LINE ( 'NONE', #3432, #2669 ) ;
#5039 = B_SPLINE_CURVE_WITH_KNOTS ( 'NONE', 3,
 ( #2721, #6911, #6807, #3530, #10080, #4387, #6041, #6144, #2067, #8410, #2825, #4532, #3630, #1914, #399, #1254, #5331, #5236, #4333, #6965, #5284, #8607, #5987, #9282, #7606, #5186, #6858, #2017, #10239, #8556, #9480, #3730, #10287, #3579, #7810, #456, #1202, #10129, #7757, #8459, #301, #7017, #2926, #1101, #4433, #8511, #4477, #1153 ),
 .UNSPECIFIED., .F., .F.,
 ( 4, 1, 1, 1, 1, 1, 1, 1, 1, 1, 1, 1, 1, 1, 1, 1, 1, 1, 1, 1, 1, 1, 1, 1, 1, 1, 1, 1, 1, 1, 1, 1, 1, 1, 1, 1, 1, 1, 1, 1, 1, 1, 1, 1, 1, 4 ),
 ( 0.000000000000000000, 0.02222222222221999915, 0.04444444444443999831, 0.06666666666666999641, 0.08888888888889000250, 0.1111111111111000027, 0.1333333333332999970, 0.1555555555555999947, 0.1777777777777999890, 0.2000000000000000111, 0.2222222222222000054, 0.2444444444443999997, 0.2666666666666999697, 0.2888888888889000195, 0.3111111111111000138, 0.3333333333333000081, 0.3555555555556000336, 0.3777777777777999724, 0.4000000000000000222, 0.4222222222221999610, 0.4444444444444000109, 0.4666666666666999808, 0.4888888888889000306, 0.5111111111110999694, 0.5333333333333000192, 0.5555555555555999891, 0.5777777777778000390, 0.5999999999999999778, 0.6222222222222000276, 0.6444444444443999664, 0.6666666666667000474, 0.6888888888888999862, 0.7111111111111000360, 0.7333333333333000859, 0.7555555555556000558, 0.7777777777777999946, 0.8000000000000000444, 0.8222222222221999832, 0.8444444444443999220, 0.8666666666667000030, 0.8888888888888999418, 0.9111111111110999916, 0.9333333333333000414, 0.9555555555556000114, 0.9777777777778000612, 1.000000000000000000 ),
 .UNSPECIFIED. ) ;
#5040 = CARTESIAN_POINT ( 'NONE',  ( 16.92248268936999978, 0.04189409840125999512, 315.0848619657999734 ) ) ;
#5041 = ORIENTED_EDGE ( 'NONE', *, *, #7378, .T. ) ;
#5042 = CARTESIAN_POINT ( 'NONE',  ( -11.03108320835583278, -10.43614982842405681, 190.9999999999995737 ) ) ;
#5043 = CARTESIAN_POINT ( 'NONE',  ( -19.56939737065003015, 2.860667089442002986, 319.5792614743400009 ) ) ;
#5044 = EDGE_LOOP ( 'NONE', ( #10246, #2862, #8412, #8978, #9696, #9672, #4163, #3434, #390, #354, #1119, #3539, #6964, #10070, #5767 ) ) ;
#5045 = CARTESIAN_POINT ( 'NONE',  ( -13.01159837870191005, -3.814965662285999759, -437.8678677476697203 ) ) ;
#5046 = CARTESIAN_POINT ( 'NONE',  ( 0.7882946689300455168, 9.499899501988618766, 315.0000000000000000 ) ) ;
#5047 = CARTESIAN_POINT ( 'NONE',  ( -11.28781796570999951, -4.951468039558000633, -285.0000000000000000 ) ) ;
#5048 = COLOUR_RGB ( '', 0.31764706, 0.68627451, 0.89019608) ;
#5049 = VERTEX_POINT ( 'NONE', #9559 ) ;
#5050 = CARTESIAN_POINT ( 'NONE',  ( -65.06086774555899410, -7.500000000000000888, -381.4479802600495759 ) ) ;
#5051 = LINE ( 'NONE', #10057, #3336 ) ;
#5052 = ADVANCED_FACE ( 'NONE', ( #1177 ), #4457, .F. ) ;
#5053 = CARTESIAN_POINT ( 'NONE',  ( -1.723960331780384880, -7.088439706543997687, -435.2349491625015503 ) ) ;
#5054 = CARTESIAN_POINT ( 'NONE',  ( -16.37727794820371585, 2.527950228764471952, -315.0000000000001137 ) ) ;
#5055 = DIRECTION ( 'NONE',  ( 0.000000000000000000, -1.000000000000000000, 0.000000000000000000 ) ) ;
#5056 = CARTESIAN_POINT ( 'NONE',  ( -26.82908671702000802, 2.500000000000000000, -441.1544246730000509 ) ) ;
#5057 = CARTESIAN_POINT ( 'NONE',  ( 9.192918156740001123, 11.10629030388999894, -316.3802825947000201 ) ) ;
#5058 = AXIS2_PLACEMENT_3D ( 'NONE', #4229, #4175, #7449 ) ;
#5059 = CARTESIAN_POINT ( 'NONE',  ( 9.231872887142856143, -4.123522793542388598, -525.3275970258257530 ) ) ;
#5060 = CARTESIAN_POINT ( 'NONE',  ( 6.750050984497039330, -5.555647561257786471, -525.3462156153834712 ) ) ;
#5061 = UNCERTAINTY_MEASURE_WITH_UNIT (LENGTH_MEASURE( 1.000000000000000082E-05 ), #9060, 'distance_accuracy_value', 'NONE');
#5062 = CARTESIAN_POINT ( 'NONE',  ( -2.000000000000000000, 4.200000000000000178, -409.5000000000000000 ) ) ;
#5063 = CARTESIAN_POINT ( 'NONE',  ( 8.666289393444031930, -8.161235200486094854, -315.0000000000000000 ) ) ;
#5064 = VERTEX_POINT ( 'NONE', #4409 ) ;
#5065 = CARTESIAN_POINT ( 'NONE',  ( 17.21226690345150701, -1.804990710747416571, -314.5172708043664898 ) ) ;
#5066 = EDGE_LOOP ( 'NONE', ( #8248, #8698 ) ) ;
#5067 = CARTESIAN_POINT ( 'NONE',  ( 12.33668477992999968, 8.731648389349999206, -317.5000000000000000 ) ) ;
#5068 = ORIENTED_EDGE ( 'NONE', *, *, #2082, .F. ) ;
#5069 = CARTESIAN_POINT ( 'NONE',  ( -0.1637764853584998959, -12.51053635490000282, -303.6197174156509391 ) ) ;
#5070 = CARTESIAN_POINT ( 'NONE',  ( 14.73022282720999598, -7.961369676960005748, -317.5770954168139610 ) ) ;
#5071 = CARTESIAN_POINT ( 'NONE',  ( -16.90171868104999930, -0.3834349726278000192, -315.0848619657999734 ) ) ;
#5072 = DIRECTION ( 'NONE',  ( 1.000000000000000000, 0.000000000000000000, 0.000000000000000000 ) ) ;
#5073 = AXIS2_PLACEMENT_3D ( 'NONE', #7156, #7899, #9787 ) ;
#5074 = CARTESIAN_POINT ( 'NONE',  ( 12.81291305286001858, 9.603378439332990624, -303.6197174156509391 ) ) ;
#5075 = CARTESIAN_POINT ( 'NONE',  ( -80.80421425739181984, -7.500000000000000000, -329.3491872523243842 ) ) ;
#5076 = ORIENTED_EDGE ( 'NONE', *, *, #6872, .T. ) ;
#5077 = CARTESIAN_POINT ( 'NONE',  ( -46.74071243416547361, -7.500000000000000000, -414.3237589990478114 ) ) ;
#5078 = LINE ( 'NONE', #5944, #9694 ) ;
#5079 = ORIENTED_EDGE ( 'NONE', *, *, #9823, .T. ) ;
#5080 = CARTESIAN_POINT ( 'NONE',  ( 20.06806562977000752, 0.4074806926876002322, 190.4207385301700128 ) ) ;
#5081 = CARTESIAN_POINT ( 'NONE',  ( 17.50000000000126832, -0.7437989020612977287, -315.0000000000001705 ) ) ;
#5082 = CARTESIAN_POINT ( 'NONE',  ( -51.61097196817823374, -12.00000000000000000, -370.6038874073401530 ) ) ;
#5083 = DIRECTION ( 'NONE',  ( 0.2896000924642900820, 0.000000000000000000, 0.9571477349106952692 ) ) ;
#5084 = CARTESIAN_POINT ( 'NONE',  ( -19.97280825118999914, -0.5561396363675005228, 191.1197171614399792 ) ) ;
#5085 = EDGE_CURVE ( 'NONE', #223, #4480, #10214, .T. ) ;
#5086 = CARTESIAN_POINT ( 'NONE',  ( 17.59298685096999648, -0.02218567204013999900, 314.4150829855000211 ) ) ;
#5087 = DIRECTION ( 'NONE',  ( 0.7784864941890657919, 0.000000000000000000, 0.6276613564377032661 ) ) ;
#5088 = CARTESIAN_POINT ( 'NONE',  ( -12.95511329522999233, -9.055231460430995583, 320.0770942683900557 ) ) ;
#5089 = CARTESIAN_POINT ( 'NONE',  ( -65.06086774555899410, -12.00000000000000000, -381.4479802600495759 ) ) ;
#5090 = DIRECTION ( 'NONE',  ( -0.8820010751365675583, 0.000000000000000000, -0.4712473909295827323 ) ) ;
#5091 = CARTESIAN_POINT ( 'NONE',  ( 16.58659719219999928, 2.947707964209000053, 314.6383426456000052 ) ) ;
#5092 = ORIENTED_EDGE ( 'NONE', *, *, #963, .F. ) ;
#5093 = CARTESIAN_POINT ( 'NONE',  ( -14.79888371878074693, -8.420183212156704400, 190.9999999999995737 ) ) ;
#5094 = ORIENTED_EDGE ( 'NONE', *, *, #7000, .T. ) ;
#5095 = CARTESIAN_POINT ( 'NONE',  ( -9.940815099545000422, 10.93780185275999983, 319.5792614743400009 ) ) ;
#5096 =( BOUNDED_CURVE ( )  B_SPLINE_CURVE ( 3, ( #8397, #5224, #1142, #10017, #5174, #6085, #2710, #6901, #1902, #188, #6797, #5120, #7647, #984, #8548, #10230, #288, #3462, #2008, #9217, #1955, #2864, #3516, #7748, #4469, #4422, #1087, #7698, #1036, #242, #4323, #3566, #341, #6135, #6847, #2056, #3621, #2658, #1850 ),
 .UNSPECIFIED., .F., .F. ) 
 B_SPLINE_CURVE_WITH_KNOTS ( ( 4, 1, 1, 1, 1, 1, 1, 1, 1, 1, 1, 1, 1, 1, 1, 1, 1, 1, 1, 1, 1, 1, 1, 1, 1, 1, 1, 1, 1, 1, 1, 1, 1, 1, 1, 1, 4 ),
 ( 0.000000000000000000, 0.03177462182248536743, 0.06473445752888724869, 0.09385364856954842017, 0.1191010430400946118, 0.1424790257418310502, 0.1662901096498168863, 0.1904342604133079375, 0.2144298290992798506, 0.2382345388122189267, 0.2620932284128464906, 0.2866356387947044948, 0.3122179111685366992, 0.3384928023102440897, 0.3654153534982623741, 0.3937977678961502859, 0.4245599715672168095, 0.4585656223635954931, 0.4952131905531249600, 0.5322445193856789603, 0.5673324073471927020, 0.5993259174520090271, 0.6288994963735405896, 0.6568908825538779528, 0.6840816459652389048, 0.7105624348628040154, 0.7360296225686681071, 0.7606150911898692524, 0.7846847747132010831, 0.8086388669220148095, 0.8327860209783324308, 0.8566619651612988884, 0.8800749352578085549, 0.9053303401216608037, 0.9344548807899611953, 0.9674420121560727281, 1.000000000000000000 ),
 .UNSPECIFIED. ) 
 CURVE ( )  GEOMETRIC_REPRESENTATION_ITEM ( )  RATIONAL_B_SPLINE_CURVE ( ( 1.171573374019466929, 1.171573374019466707, 1.171573374019466929, 1.171573374019466929, 1.171573374019466929, 1.171573374019466929, 1.171573374019466929, 1.171573374019466929, 1.171573374019466929, 1.171573374019466929, 1.171573374019466929, 1.171573374019466929, 1.171573374019466929, 1.171573374019466929, 1.171573374019466929, 1.171573374019466929, 1.171573374019466929, 1.171573374019466929, 1.171573374019466929, 1.171573374019466929, 1.171573374019466929, 1.171573374019466929, 1.171573374019466929, 1.171573374019466929, 1.171573374019466929, 1.171573374019466929, 1.171573374019466929, 1.171573374019466929, 1.171573374019466929, 1.171573374019466929, 1.171573374019466929, 1.171573374019466929, 1.171573374019466929, 1.171573374019466929, 1.171573374019466929, 1.171573374019466929, 1.171573374019466929, 1.171573374019466929, 1.171573374019466929 ) ) 
 REPRESENTATION_ITEM ( '' )  );
#5097 = ADVANCED_FACE ( 'NONE', ( #2042 ), #8582, .T. ) ;
#5098 =( REPRESENTATION_RELATIONSHIP ('NONE','NONE', #8468, #1806 ) REPRESENTATION_RELATIONSHIP_WITH_TRANSFORMATION ( #8381 )SHAPE_REPRESENTATION_RELATIONSHIP( ) );
#5099 = EDGE_CURVE ( 'NONE', #1416, #7593, #933, .T. ) ;
#5100 = CARTESIAN_POINT ( 'NONE',  ( -9.752548285928396510, -3.766234771432999562, -438.4914339879979366 ) ) ;
#5101 = CARTESIAN_POINT ( 'NONE',  ( -2.257382111677873393, 9.415175415973715545, 315.0000000000000000 ) ) ;
#5102 = CARTESIAN_POINT ( 'NONE',  ( -43.46674421124934184, -9.000000000000001776, -402.7790142173016648 ) ) ;
#5103 = ORIENTED_EDGE ( 'NONE', *, *, #138, .T. ) ;
#5104 = CARTESIAN_POINT ( 'NONE',  ( 18.86992372454000133, -1.611776198549999872, -302.4999999999529905 ) ) ;
#5105 =( LENGTH_UNIT ( ) NAMED_UNIT ( * ) SI_UNIT ( .MILLI., .METRE. ) );
#5106 = CARTESIAN_POINT ( 'NONE',  ( -13.28926923829693152, -6.170678168660001184, -437.9230910759725930 ) ) ;
#5107 = CARTESIAN_POINT ( 'NONE',  ( 17.44869542667227691, -0.8969788568403171958, 314.4999390965244288 ) ) ;
#5108 = CARTESIAN_POINT ( 'NONE',  ( -28.01838671672000203, 2.500000000000000000, -497.7560445212000104 ) ) ;
#5109 = CARTESIAN_POINT ( 'NONE',  ( -79.31727611502927289, -2.500000000000000000, -351.2304352734219606 ) ) ;
#5110 = AXIS2_PLACEMENT_3D ( 'NONE', #6999, #10271, #5366 ) ;
#5111 = FACE_OUTER_BOUND ( 'NONE', #1311, .T. ) ;
#5112 = EDGE_CURVE ( 'NONE', #1530, #9641, #2364, .T. ) ;
#5113 = CARTESIAN_POINT ( 'NONE',  ( 8.350293318704649081, -4.249850286232732088, -525.7107168166273823 ) ) ;
#5114 = B_SPLINE_CURVE_WITH_KNOTS ( 'NONE', 3,
 ( #9683, #446, #9578, #10326 ),
 .UNSPECIFIED., .F., .F.,
 ( 4, 4 ),
 ( 0.000000000000000000, 1.000000000000000000 ),
 .UNSPECIFIED. ) ;
#5115 = CARTESIAN_POINT ( 'NONE',  ( 7.450340645337907297, -5.634999222355125070, -525.6669455952093131 ) ) ;
#5116 = CARTESIAN_POINT ( 'NONE',  ( -12.99025666465511009, -6.750000000004000356, -438.9652312646727523 ) ) ;
#5117 = CARTESIAN_POINT ( 'NONE',  ( 5.242074483217282754, -9.033702059254418160, -314.9999999999999432 ) ) ;
#5118 = ORIENTED_EDGE ( 'NONE', *, *, #8123, .T. ) ;
#5119 = CARTESIAN_POINT ( 'NONE',  ( 17.50000000000000000, 0.000000000000000000, -314.4999343908002629 ) ) ;
#5120 = CARTESIAN_POINT ( 'NONE',  ( 11.75848697160781064, -10.12394145745024687, -316.5000000000004547 ) ) ;
#5121 = VERTEX_POINT ( 'NONE', #7358 ) ;
#5122 = CARTESIAN_POINT ( 'NONE',  ( -17.62858316411999837, 4.302404616280000482, -317.5000000000030127 ) ) ;
#5123 = EDGE_LOOP ( 'NONE', ( #9174, #6405, #7867, #1687 ) ) ;
#5124 = CYLINDRICAL_SURFACE ( 'NONE', #6944, 29.99999999999999289 ) ;
#5125 = CARTESIAN_POINT ( 'NONE',  ( 18.93734960604998463, -3.176822791883000985, -317.5770954168139610 ) ) ;
#5126 = DIRECTION ( 'NONE',  ( 0.000000000000000000, -0.000000000000000000, -1.000000000000000000 ) ) ;
#5127 = CARTESIAN_POINT ( 'NONE',  ( 0.000000000000000000, 0.000000000000000000, 0.000000000000000000 ) ) ;
#5128 = CARTESIAN_POINT ( 'NONE',  ( -14.97309261602000419, 8.296494983500004139, -303.6197174156520759 ) ) ;
#5129 = CARTESIAN_POINT ( 'NONE',  ( -6.176342266831065686, -9.366307616516619916, 314.4999456809351273 ) ) ;
#5130 = ORIENTED_EDGE ( 'NONE', *, *, #3790, .F. ) ;
#5131 = DIRECTION ( 'NONE',  ( 0.000000000000000000, 0.000000000000000000, -1.000000000000000000 ) ) ;
#5132 = CARTESIAN_POINT ( 'NONE',  ( -2.907097610887497741, -7.500000000000000888, -345.9038247371837542 ) ) ;
#5133 = VERTEX_POINT ( 'NONE', #3273 ) ;
#5134 = CARTESIAN_POINT ( 'NONE',  ( 4.867894159875999271, -12.21747625305000007, 190.4207385301700128 ) ) ;
#5135 = LINE ( 'NONE', #6701, #8630 ) ;
#5136 = CARTESIAN_POINT ( 'NONE',  ( -27.92645732311634532, -9.000000000000001776, -417.8271580078818488 ) ) ;
#5137 = CARTESIAN_POINT ( 'NONE',  ( -18.17619403612001250, 5.223318733890998544, 191.1197171614399792 ) ) ;
#5138 = MANIFOLD_SOLID_BREP ( 'Stock-MAS-686-1', #2481 ) ;
#5139 = AXIS2_PLACEMENT_3D ( 'NONE', #2334, #871, #3243 ) ;
#5140 = AXIS2_PLACEMENT_3D ( 'NONE', #3505, #380, #8335 ) ;
#5141 = EDGE_CURVE ( 'NONE', #6958, #223, #10372, .T. ) ;
#5142 = CARTESIAN_POINT ( 'NONE',  ( 16.41165915566000066, -2.800979832323999830, 314.8616023057000461 ) ) ;
#5143 = PLANE ( 'NONE',  #3817 ) ;
#5144 = CARTESIAN_POINT ( 'NONE',  ( 19.37251270682998694, -1.820313540576997680, 320.0770942683900557 ) ) ;
#5145 = CARTESIAN_POINT ( 'NONE',  ( -3.206477623445924685, 9.870911232215625830, 314.4999441614609736 ) ) ;
#5146 = CARTESIAN_POINT ( 'NONE',  ( 8.032401884333960851, 11.45915766226284482, -303.4999999999990905 ) ) ;
#5147 = CARTESIAN_POINT ( 'NONE',  ( 14.52969073417999901, 5.422537850045999974, 314.6383426456000052 ) ) ;
#5148 = ORIENTED_EDGE ( 'NONE', *, *, #9381, .T. ) ;
#5149 = CARTESIAN_POINT ( 'NONE',  ( -102.0103468492230547, -7.500000000000000000, -289.6591388711787545 ) ) ;
#5150 = CARTESIAN_POINT ( 'NONE',  ( 3.213253768582002845, 12.43294388789000138, 319.5792614743400009 ) ) ;
#5151 = CIRCLE ( 'NONE', #520, 3.499999999999997335 ) ;
#5152 = ADVANCED_FACE ( 'NONE', ( #6551 ), #8726, .T. ) ;
#5153 = CARTESIAN_POINT ( 'NONE',  ( -2.240834826158499382, -2.262508910126998174, -436.4488545418295757 ) ) ;
#5154 = AXIS2_PLACEMENT_3D ( 'NONE', #2299, #9822, #4828 ) ;
#5155 = CARTESIAN_POINT ( 'NONE',  ( -2.158263635479988896, 9.422507356620213770, 315.0000000000001137 ) ) ;
#5156 = DIRECTION ( 'NONE',  ( 0.000000000000000000, -1.000000000000000000, 0.000000000000000000 ) ) ;
#5157 = ORIENTED_EDGE ( 'NONE', *, *, #7529, .T. ) ;
#5158 = COLOUR_RGB ( '', 0.66274510, 0.83137255, 0.94901961) ;
#5159 = CARTESIAN_POINT ( 'NONE',  ( 16.90628502044000214, -5.238535436438000126, -302.5000000000009663 ) ) ;
#5160 = DIRECTION ( 'NONE',  ( 0.000000000000000000, 0.000000000000000000, -1.000000000000000000 ) ) ;
#5161 = CARTESIAN_POINT ( 'NONE',  ( -4.263294926846636912, -7.373286713554001892, -435.4918557313383758 ) ) ;
#5162 = EDGE_CURVE ( 'NONE', #1953, #4467, #1388, .T. ) ;
#5163 = CARTESIAN_POINT ( 'NONE',  ( -14.89798725392377321, 4.565017050278197708, -315.0000000000000568 ) ) ;
#5164 = CARTESIAN_POINT ( 'NONE',  ( 8.506801009283002202, 10.15345907998999486, 190.0071920248299477 ) ) ;
#5165 = CARTESIAN_POINT ( 'NONE',  ( -28.01838671672000203, -2.500000000000000000, -497.7560445212000104 ) ) ;
#5166 = CARTESIAN_POINT ( 'NONE',  ( -16.17578790646000186, -7.500000000000000000, -433.5685902625999688 ) ) ;
#5167 = CARTESIAN_POINT ( 'NONE',  ( -1.108984404642836541, -7.422390432154000628, -435.0786752202253638 ) ) ;
#5168 = UNCERTAINTY_MEASURE_WITH_UNIT (LENGTH_MEASURE( 1.000000000000000082E-05 ), #9021, 'distance_accuracy_value', 'NONE');
#5169 = DIRECTION ( 'NONE',  ( 0.000000000000000000, -1.000000000000000000, 0.000000000000000000 ) ) ;
#5170 = BREP_WITH_VOIDS ( 'NONE', #8143, ( #100, #8823 ) );
#5171 = ORIENTED_EDGE ( 'NONE', *, *, #10479, .F. ) ;
#5172 = B_SPLINE_CURVE_WITH_KNOTS ( 'NONE', 3,
 ( #8054, #2421, #8974, #1616, #3972, #7255, #9727, #5633, #9834, #7361, #4084, #4836, #1831 ),
 .UNSPECIFIED., .F., .F.,
 ( 4, 1, 1, 1, 1, 1, 1, 1, 1, 1, 4 ),
 ( 0.000000000000000000, 0.08333333333333001192, 0.1666666666667000196, 0.2500000000000000000, 0.3333333333333000081, 0.5000000000000000000, 0.6666666666667000474, 0.7500000000000000000, 0.8333333333333000637, 0.9166666666667000474, 1.000000000000000000 ),
 .UNSPECIFIED. ) ;
#5173 = CARTESIAN_POINT ( 'NONE',  ( 1.281333103385001726, 11.37293729856000368, 319.9928079742500131 ) ) ;
#5174 = CARTESIAN_POINT ( 'NONE',  ( 18.56670159326493064, -4.707099758006331847, -316.5000000000004547 ) ) ;
#5175 = EDGE_LOOP ( 'NONE', ( #6756, #1363 ) ) ;
#5176 = DIRECTION ( 'NONE',  ( -0.1071946444232961260, 0.000000000000000000, 0.9942380540931650135 ) ) ;
#5177 = ORIENTED_EDGE ( 'NONE', *, *, #2590, .T. ) ;
#5178 = CARTESIAN_POINT ( 'NONE',  ( -10.19016500772999656, 9.569509725303996461, -317.4928077629770087 ) ) ;
#5179 = CARTESIAN_POINT ( 'NONE',  ( 16.88563860788000781, -5.080169144092001154, -317.4928077629770087 ) ) ;
#5180 = SHAPE_REPRESENTATION ( 'Handle Mounting Bracket', ( #2817 ), #6445 ) ;
#5181 = VECTOR ( 'NONE', #9561, 1000.000000000000114 ) ;
#5182 = CARTESIAN_POINT ( 'NONE',  ( -17.18263598829999950, 2.199757124398999952, -314.4150829855000211 ) ) ;
#5183 = DIRECTION ( 'NONE',  ( 1.000000000000000000, 0.000000000000000000, 0.000000000000000000 ) ) ;
#5184 = CARTESIAN_POINT ( 'NONE',  ( -9.995120163707431615, -8.217201912095820404, 314.4999464406706693 ) ) ;
#5185 = ORIENTED_EDGE ( 'NONE', *, *, #641, .T. ) ;
#5186 = CARTESIAN_POINT ( 'NONE',  ( -2.585384220735000405, -11.41066401029999966, 190.0000000000000000 ) ) ;
#5187 = CARTESIAN_POINT ( 'NONE',  ( -19.99996733365994928, -0.3063832366037745891, 319.0000000000003979 ) ) ;
#5188 = VERTEX_POINT ( 'NONE', #2573 ) ;
#5189 = CARTESIAN_POINT ( 'NONE',  ( -2.000000000000000000, 2.500000000000000000, -413.0000000000000000 ) ) ;
#5190 = LINE ( 'NONE', #3316, #5888 ) ;
#5191 = DIRECTION ( 'NONE',  ( 0.000000000000000000, 1.000000000000000000, 0.000000000000000000 ) ) ;
#5192 = CARTESIAN_POINT ( 'NONE',  ( 20.06711733022002164, -0.4206966322103001255, 190.4207385301700128 ) ) ;
#5193 = VECTOR ( 'NONE', #5087, 999.9999999999998863 ) ;
#5194 = CARTESIAN_POINT ( 'NONE',  ( -0.5105614201597979962, -7.485013515304997256, -434.2009872517302256 ) ) ;
#5195 = LINE ( 'NONE', #7512, #4341 ) ;
#5196 = AXIS2_PLACEMENT_3D ( 'NONE', #6142, #397, #298 ) ;
#5197 = CARTESIAN_POINT ( 'NONE',  ( 19.19790409518002861, -3.716965664678998582, 319.5792614743400009 ) ) ;
#5198 = CARTESIAN_POINT ( 'NONE',  ( -19.68871134463705985, -7.500000000000000888, -416.4361005590961327 ) ) ;
#5199 = CARTESIAN_POINT ( 'NONE',  ( 16.21525914616999842, -2.693567875512000054, -315.0848619657999734 ) ) ;
#5200 = CARTESIAN_POINT ( 'NONE',  ( -10.58688533405000065, 7.844683714540999553, 314.6383426456000052 ) ) ;
#5201 = ORIENTED_EDGE ( 'NONE', *, *, #6274, .T. ) ;
#5202 = CARTESIAN_POINT ( 'NONE',  ( 16.34529002343605697, -7.216405960070772174, 190.9999999999995737 ) ) ;
#5203 = CARTESIAN_POINT ( 'NONE',  ( 20.00482943604999164, 0.07455149923640995435, 318.8802828394900644 ) ) ;
#5204 = CARTESIAN_POINT ( 'NONE',  ( -11.92907573672570720, -3.757347598437999370, -437.6506565322029019 ) ) ;
#5205 = CARTESIAN_POINT ( 'NONE',  ( 9.619189022994751426, 7.822639675800805215, 315.0000000000000000 ) ) ;
#5206 = CARTESIAN_POINT ( 'NONE',  ( -17.50000003227012613, 5.857864393370422640, 314.9999999999999432 ) ) ;
#5207 = CARTESIAN_POINT ( 'NONE',  ( -6.492778508125761405, -3.359043026927307274, -437.1259979785785958 ) ) ;
#5208 = FILL_AREA_STYLE_COLOUR ( '', #3159 ) ;
#5209 = STYLED_ITEM ( 'NONE', ( #8160 ), #4657 ) ;
#5210 = CARTESIAN_POINT ( 'NONE',  ( -77.77979771402830522, -7.500000000000000000, -385.9384419754180158 ) ) ;
#5211 = VECTOR ( 'NONE', #6365, 1000.000000000000000 ) ;
#5212 = CARTESIAN_POINT ( 'NONE',  ( -16.03969916442341415, 3.142024325209860081, -314.9999999999999432 ) ) ;
#5213 = FACE_OUTER_BOUND ( 'NONE', #6845, .T. ) ;
#5214 = CARTESIAN_POINT ( 'NONE',  ( -1.742616259932011413, -2.630534087998720683, -434.8631598522362083 ) ) ;
#5215 = CIRCLE ( 'NONE', #1442, 0.5000000000000004441 ) ;
#5216 = DIRECTION ( 'NONE',  ( 0.000000000000000000, 1.000000000000000000, 0.000000000000000000 ) ) ;
#5217 = EDGE_CURVE ( 'NONE', #2675, #10018, #1825, .T. ) ;
#5218 = VECTOR ( 'NONE', #4951, 1000.000000000000000 ) ;
#5219 = DIRECTION ( 'NONE',  ( 0.9712267471052594692, 0.000000000000000000, 0.2381566831044984456 ) ) ;
#5220 = CYLINDRICAL_SURFACE ( 'NONE', #8557, 3.500000000000003109 ) ;
#5221 = EDGE_CURVE ( 'NONE', #2124, #8515, #5038, .T. ) ;
#5222 = ORIENTED_EDGE ( 'NONE', *, *, #2992, .F. ) ;
#5223 = DIRECTION ( 'NONE',  ( 0.000000000000000000, 1.000000000000000000, -0.000000000000000000 ) ) ;
#5224 = CARTESIAN_POINT ( 'NONE',  ( 19.99979366059626074, -0.5741561031401761772, -316.5000000000005684 ) ) ;
#5225 = CARTESIAN_POINT ( 'NONE',  ( -2.000000000000000000, 2.500000000000000000, -406.0000000000000000 ) ) ;
#5226 = ORIENTED_EDGE ( 'NONE', *, *, #8269, .T. ) ;
#5227 = CIRCLE ( 'NONE', #426, 3.500000000000003997 ) ;
#5228 = CARTESIAN_POINT ( 'NONE',  ( -18.90091799877999179, 0.2928069713013998765, -317.4928077629770087 ) ) ;
#5229 = CONICAL_SURFACE ( 'NONE', #603, 3.400000000000014122, 0.7853981633975631871 ) ;
#5230 = CARTESIAN_POINT ( 'NONE',  ( -18.92046274781997894, -3.214434834450002221, -317.5770954168139610 ) ) ;
#5231 = ADVANCED_FACE ( 'NONE', ( #10044 ), #8158, .T. ) ;
#5232 = DIRECTION ( 'NONE',  ( -0.000000000000000000, 1.000000000000000000, 0.000000000000000000 ) ) ;
#5233 = EDGE_CURVE ( 'NONE', #5378, #4852, #1215, .T. ) ;
#5234 = DIRECTION ( 'NONE',  ( 0.4712473909295827323, 0.000000000000000000, -0.8820010751365675583 ) ) ;
#5235 = ORIENTED_EDGE ( 'NONE', *, *, #7135, .F. ) ;
#5236 = CARTESIAN_POINT ( 'NONE',  ( 9.801682940292002044, -9.841837802148999614, 190.0000000000000000 ) ) ;
#5237 = CARTESIAN_POINT ( 'NONE',  ( -19.96236207922240879, -0.9438262771025411890, 319.0000000000003979 ) ) ;
#5238 = APPLICATION_CONTEXT ( 'automotive_design' ) ;
#5239 = EDGE_LOOP ( 'NONE', ( #5666, #9783, #8025, #1578 ) ) ;
#5240 = CARTESIAN_POINT ( 'NONE',  ( -19.99979366059625718, 0.5741561031401783977, -316.5000000000005116 ) ) ;
#5241 = ORIENTED_EDGE ( 'NONE', *, *, #4259, .T. ) ;
#5242 = CYLINDRICAL_SURFACE ( 'NONE', #1618, 3.500000000000003109 ) ;
#5243 = LINE ( 'NONE', #9437, #6689 ) ;
#5244 = DIRECTION ( 'NONE',  ( 0.000000000000000000, -1.000000000000000000, 0.000000000000000000 ) ) ;
#5245 = EDGE_CURVE ( 'NONE', #9105, #8720, #9920, .T. ) ;
#5246 = DIRECTION ( 'NONE',  ( -0.4712473909295827323, 0.000000000000000000, 0.8820010751365675583 ) ) ;
#5247 = DIRECTION ( 'NONE',  ( 0.000000000000000000, -1.000000000000000000, 0.000000000000000000 ) ) ;
#5248 = CARTESIAN_POINT ( 'NONE',  ( 7.514439085588995759, -11.67576679883001667, 319.5792614743400009 ) ) ;
#5249 = CARTESIAN_POINT ( 'NONE',  ( 16.41165915566000066, -2.800979832323999830, -314.8616023057000461 ) ) ;
#5250 = CARTESIAN_POINT ( 'NONE',  ( -10.67587555525000020, 8.049811041412000989, 314.4150829855000211 ) ) ;
#5251 = VERTEX_POINT ( 'NONE', #10197 ) ;
#5252 = CARTESIAN_POINT ( 'NONE',  ( 12.57201637590000942, -8.467554047266999007, 190.0071920248299477 ) ) ;
#5253 = EDGE_LOOP ( 'NONE', ( #9350, #257, #4808, #6185 ) ) ;
#5254 = CARTESIAN_POINT ( 'NONE',  ( 12.21300849950000433, 9.900542285453001412, 318.8802828394900644 ) ) ;
#5255 = SURFACE_SIDE_STYLE ('',( #8316 ) ) ;
#5256 = CARTESIAN_POINT ( 'NONE',  ( -17.56970546055000071, 0.4338786413876999926, 314.4150829855000211 ) ) ;
#5257 = CARTESIAN_POINT ( 'NONE',  ( -16.13945612244922501, 2.966804785441415238, 314.9999999999999432 ) ) ;
#5258 = EDGE_CURVE ( 'NONE', #3896, #10437, #4603, .T. ) ;
#5259 = CARTESIAN_POINT ( 'NONE',  ( 15.00000000000325961, 7.547804830080786473E-15, 315.0000000000001705 ) ) ;
#5260 = CARTESIAN_POINT ( 'NONE',  ( -4.094888478148218880, -3.021466021405220914, -436.2739009261703131 ) ) ;
#5261 = CARTESIAN_POINT ( 'NONE',  ( -11.73256627085759973, -5.797438927934700281, -438.1636576033711776 ) ) ;
#5262 = CARTESIAN_POINT ( 'NONE',  ( -16.45380452100018687, 2.370995337294541816, -315.0000000000000568 ) ) ;
#5263 = CARTESIAN_POINT ( 'NONE',  ( 9.595833218033995138, 9.789665514059997520, 190.0071920248299477 ) ) ;
#5264 = DIRECTION ( 'NONE',  ( -0.2728306852452879183, 0.000000000000000000, -0.9620620651437133963 ) ) ;
#5265 = CARTESIAN_POINT ( 'NONE',  ( -19.00000000000000000, 0.000000000000000000, -317.4999999998989892 ) ) ;
#5266 = ADVANCED_FACE ( 'NONE', ( #2134 ), #4446, .T. ) ;
#5267 = CARTESIAN_POINT ( 'NONE',  ( 6.280112539859566745, -5.511129512251558893, -524.8290735491510759 ) ) ;
#5268 = CARTESIAN_POINT ( 'NONE',  ( 13.94549574055089458, -5.407931305651876741, 315.0000000000001137 ) ) ;
#5269 = CARTESIAN_POINT ( 'NONE',  ( -12.07130791617000121, 6.858215270785999351, -314.8616023057000461 ) ) ;
#5270 = ORIENTED_EDGE ( 'NONE', *, *, #1160, .F. ) ;
#5271 = VECTOR ( 'NONE', #1182, 1000.000000000000000 ) ;
#5272 = CARTESIAN_POINT ( 'NONE',  ( -9.539154743984001428, 9.809959732869000248, 319.9928079742500131 ) ) ;
#5273 = CARTESIAN_POINT ( 'NONE',  ( -14.98500449093754483, -3.491150269972000064, -438.4247239981262396 ) ) ;
#5274 = CARTESIAN_POINT ( 'NONE',  ( -37.57635160138833896, -7.500000000000000888, -403.2777420460153053 ) ) ;
#5275 = ORIENTED_EDGE ( 'NONE', *, *, #5348, .T. ) ;
#5276 = CARTESIAN_POINT ( 'NONE',  ( 6.235150775465998052, 10.74512744517000407, -317.4928077629770087 ) ) ;
#5277 = ADVANCED_FACE ( 'NONE', ( #6056 ), #7691, .F. ) ;
#5278 = CARTESIAN_POINT ( 'NONE',  ( 3.772811979575000141, -12.36790329786001763, -317.0792622552969533 ) ) ;
#5279 = EDGE_CURVE ( 'NONE', #3553, #6229, #6960, .T. ) ;
#5280 = CARTESIAN_POINT ( 'NONE',  ( 17.19853431800999743, -2.231396706187000145, -315.0000000000000000 ) ) ;
#5281 = AXIS2_PLACEMENT_3D ( 'NONE', #9212, #5973, #9266 ) ;
#5282 = LINE ( 'NONE', #8554, #2108 ) ;
#5283 = ORIENTED_EDGE ( 'NONE', *, *, #7709, .F. ) ;
#5284 = CARTESIAN_POINT ( 'NONE',  ( 6.280550016735999996, -10.85821747223999978, 190.0000000000000000 ) ) ;
#5285 = CARTESIAN_POINT ( 'NONE',  ( -18.21047658595729857, -5.188723016677323052, 319.0000000000003979 ) ) ;
#5286 = EDGE_LOOP ( 'NONE', ( #3040, #2558, #5103, #9435 ) ) ;
#5287 = CARTESIAN_POINT ( 'NONE',  ( -17.02428600387000301, -6.565037456673000982, 191.1197171614399792 ) ) ;
#5288 = VERTEX_POINT ( 'NONE', #10028 ) ;
#5289 = DIRECTION ( 'NONE',  ( 0.000000000000000000, 0.000000000000000000, -1.000000000000000000 ) ) ;
#5290 = CARTESIAN_POINT ( 'NONE',  ( -16.85751871341000907, -5.113642021703998175, -302.5071922382879279 ) ) ;
#5291 = ADVANCED_FACE ( 'NONE', ( #789 ), #1751, .F. ) ;
#5292 = CARTESIAN_POINT ( 'NONE',  ( -39.23786858994942151, -9.000000000000001776, -387.8670522075712483 ) ) ;
#5293 = CARTESIAN_POINT ( 'NONE',  ( -0.5691292782512946680, -7.474371670585999716, -434.2981779884299272 ) ) ;
#5294 =( NAMED_UNIT ( * ) SI_UNIT ( $, .STERADIAN. ) SOLID_ANGLE_UNIT ( ) );
#5295 = CARTESIAN_POINT ( 'NONE',  ( -3.306880204566999382, 11.21686954173999951, -302.5071922382879279 ) ) ;
#5296 = CARTESIAN_POINT ( 'NONE',  ( -17.04162109443001683, -6.546751591322998109, 318.8802828394900644 ) ) ;
#5297 = CARTESIAN_POINT ( 'NONE',  ( 17.56954514911999965, 0.4333932196220999788, -314.4150829855000211 ) ) ;
#5298 = CARTESIAN_POINT ( 'NONE',  ( -4.061138133959000029, 9.851562218542998295, 314.4150829855000211 ) ) ;
#5299 = EDGE_LOOP ( 'NONE', ( #304, #2906, #5118, #1429 ) ) ;
#5300 = CARTESIAN_POINT ( 'NONE',  ( -2.556522775252001445, -11.29259618907000196, 190.0071920248299477 ) ) ;
#5301 = VERTEX_POINT ( 'NONE', #2672 ) ;
#5302 = CARTESIAN_POINT ( 'NONE',  ( -11.98520373079999679, 10.00909632395999438, 318.8802828394900644 ) ) ;
#5303 = DIRECTION ( 'NONE',  ( -1.000000000000000000, 0.000000000000000000, 0.000000000000000000 ) ) ;
#5304 = CIRCLE ( 'NONE', #8915, 12.50000000000002309 ) ;
#5305 = DIRECTION ( 'NONE',  ( 0.000000000000000000, -1.000000000000000000, 0.000000000000000000 ) ) ;
#5306 = CARTESIAN_POINT ( 'NONE',  ( -28.01838671672410896, -2.500000000000000000, -497.7560445212019999 ) ) ;
#5307 = CARTESIAN_POINT ( 'NONE',  ( -14.79012398733999767, -1.483731117707002278, -284.9999999999999432 ) ) ;
#5308 = VECTOR ( 'NONE', #7293, 1000.000000000000000 ) ;
#5309 = CARTESIAN_POINT ( 'NONE',  ( -15.88699210612483981, -3.373196549223931306, -314.9999999999999432 ) ) ;
#5310 = CARTESIAN_POINT ( 'NONE',  ( -10.01353696546765804, -3.849175066121115485, -438.2031691364160793 ) ) ;
#5311 = CARTESIAN_POINT ( 'NONE',  ( 17.33328289455321425, 2.867118450878387397E-08, 314.6666162271451981 ) ) ;
#5312 = DIRECTION ( 'NONE',  ( -0.9997724835175819669, 0.000000000000000000, 0.02133028834981342756 ) ) ;
#5313 = CARTESIAN_POINT ( 'NONE',  ( -10.54249803899487326, 7.451732067202640586, -315.0000000000000000 ) ) ;
#5314 = CARTESIAN_POINT ( 'NONE',  ( 14.91611818836001824, 6.947523351336002406, 190.0071920248299477 ) ) ;
#5315 = DIRECTION ( 'NONE',  ( 0.9921831154218023752, -0.000000000000000000, 0.1247904863035890627 ) ) ;
#5316 = CARTESIAN_POINT ( 'NONE',  ( -1.614076495133000000, -11.47540331082000087, -317.5000000000000000 ) ) ;
#5317 = CARTESIAN_POINT ( 'NONE',  ( 19.00000000000000000, 0.000000000000000000, -317.4999999998989892 ) ) ;
#5318 = CARTESIAN_POINT ( 'NONE',  ( 13.67632236045006167, -5.618997091738346050, 315.0000000000000000 ) ) ;
#5319 = CARTESIAN_POINT ( 'NONE',  ( -11.96281778373999849, 6.662668310474999522, -315.0848619657999734 ) ) ;
#5320 = FACE_OUTER_BOUND ( 'NONE', #5025, .T. ) ;
#5321 = DIRECTION ( 'NONE',  ( 0.000000000000000000, 1.000000000000000000, -0.000000000000000000 ) ) ;
#5322 = FACE_OUTER_BOUND ( 'NONE', #4244, .T. ) ;
#5323 = EDGE_LOOP ( 'NONE', ( #1847, #1467, #1152, #3770 ) ) ;
#5324 = CARTESIAN_POINT ( 'NONE',  ( 11.21026319665000948, 9.143022107836994650, -317.4928077629770087 ) ) ;
#5325 = ADVANCED_FACE ( 'NONE', ( #5022 ), #944, .F. ) ;
#5326 = CARTESIAN_POINT ( 'NONE',  ( 5.336288444022999400, -12.13785676344998699, -317.0792622552969533 ) ) ;
#5327 = LINE ( 'NONE', #6190, #7681 ) ;
#5328 = ADVANCED_FACE ( 'NONE', ( #995 ), #5724, .F. ) ;
#5329 = CARTESIAN_POINT ( 'NONE',  ( 17.44177680037102007, 0.9115828329869209989, -314.5029970719331232 ) ) ;
#5330 = ORIENTED_EDGE ( 'NONE', *, *, #5085, .F. ) ;
#5331 = CARTESIAN_POINT ( 'NONE',  ( 10.77777196380999847, -9.457622649256999026, 190.0000000000000000 ) ) ;
#5332 = EDGE_CURVE ( 'NONE', #8095, #9479, #2836, .T. ) ;
#5333 = CARTESIAN_POINT ( 'NONE',  ( -19.99999036626000048, -4.642009783819999925E-09, -316.5000000000000000 ) ) ;
#5334 = VERTEX_POINT ( 'NONE', #9065 ) ;
#5335 = ORIENTED_EDGE ( 'NONE', *, *, #1454, .T. ) ;
#5336 = CARTESIAN_POINT ( 'NONE',  ( -5.563766465756743607, -8.000000000000000000, -337.3048648817380126 ) ) ;
#5337 = CARTESIAN_POINT ( 'NONE',  ( 7.636686903722000430, -10.40663048292000070, -302.5071922382879279 ) ) ;
#5338 = CARTESIAN_POINT ( 'NONE',  ( 18.70579689905999032, 4.435290649195002821, 191.1197171614399792 ) ) ;
#5339 = VECTOR ( 'NONE', #305, 1000.000000000000000 ) ;
#5340 = CARTESIAN_POINT ( 'NONE',  ( -1.136797867647343807, -7.487797410750999028, -434.4157425830155717 ) ) ;
#5341 = SURFACE_STYLE_USAGE ( .BOTH. , #7926 ) ;
#5342 = EDGE_CURVE ( 'NONE', #3089, #8136, #4210, .T. ) ;
#5343 = CARTESIAN_POINT ( 'NONE',  ( 18.77308876972001173, 1.495304374661000413, -302.5071922382879279 ) ) ;
#5344 = CARTESIAN_POINT ( 'NONE',  ( -19.14248421182001891, -3.638193899013998145, 318.8802828394900644 ) ) ;
#5345 = VECTOR ( 'NONE', #3665, 1000.000000000000000 ) ;
#5346 = CARTESIAN_POINT ( 'NONE',  ( 17.36938240862999905, -0.02134527931160000100, -314.6383426456000052 ) ) ;
#5347 = CARTESIAN_POINT ( 'NONE',  ( -16.92217352393999974, 0.01966449385449000123, 315.0848619657999734 ) ) ;
#5348 = EDGE_CURVE ( 'NONE', #6305, #9271, #5935, .T. ) ;
#5349 = AXIS2_PLACEMENT_3D ( 'NONE', #3053, #2361, #2303 ) ;
#5350 = VERTEX_POINT ( 'NONE', #1967 ) ;
#5351 = DIRECTION ( 'NONE',  ( 0.000000000000000000, 1.000000000000000000, -0.000000000000000000 ) ) ;
#5352 = CARTESIAN_POINT ( 'NONE',  ( -0.6929407895232514436, -7.497116523641391694, -434.2160164714800317 ) ) ;
#5353 = DIRECTION ( 'NONE',  ( 0.9712267471052612455, 0.000000000000000000, 0.2381566831044910626 ) ) ;
#5354 = EDGE_CURVE ( 'NONE', #4571, #2720, #5039, .T. ) ;
#5355 = VECTOR ( 'NONE', #9404, 1000.000000000000000 ) ;
#5356 = LINE ( 'NONE', #9354, #3917 ) ;
#5357 = CARTESIAN_POINT ( 'NONE',  ( 18.78897325516000194, 1.756194273835000041, 320.0000000000000000 ) ) ;
#5358 = CARTESIAN_POINT ( 'NONE',  ( 15.00000000000072120, -0.4945770392355430256, -284.9999999999999432 ) ) ;
#5359 = CARTESIAN_POINT ( 'NONE',  ( -3.800715135322751514, -2.979668659210926940, -436.1572919893235962 ) ) ;
#5360 = PLANE ( 'NONE',  #4529 ) ;
#5361 = CARTESIAN_POINT ( 'NONE',  ( -7.533731257138555293, -6.615200789007997351, -438.0078122065712023 ) ) ;
#5362 = CARTESIAN_POINT ( 'NONE',  ( 4.532042191365901473, 9.152867265080528725, -315.0000000000000568 ) ) ;
#5363 = DIRECTION ( 'NONE',  ( 0.000000000000000000, 1.000000000000000000, 0.000000000000000000 ) ) ;
#5364 = CARTESIAN_POINT ( 'NONE',  ( 17.16660215780888166, 1.253876006774286806E-08, -314.8332688233516024 ) ) ;
#5365 = ORIENTED_EDGE ( 'NONE', *, *, #9764, .T. ) ;
#5366 = DIRECTION ( 'NONE',  ( 0.2728306852451984343, 0.000000000000000000, 0.9620620651437388204 ) ) ;
#5367 = PLANE ( 'NONE',  #316 ) ;
#5368 = EDGE_CURVE ( 'NONE', #8790, #9887, #7708, .T. ) ;
#5369 =( GEOMETRIC_REPRESENTATION_CONTEXT ( 3 ) GLOBAL_UNCERTAINTY_ASSIGNED_CONTEXT ( ( #128 ) ) GLOBAL_UNIT_ASSIGNED_CONTEXT ( ( #4984, #4882, #5733 ) ) REPRESENTATION_CONTEXT ( 'NONE', 'WORKASPACE' ) );
#5370 = CARTESIAN_POINT ( 'NONE',  ( 0.000000000000000000, 0.000000000000000000, 0.000000000000000000 ) ) ;
#5371 = CARTESIAN_POINT ( 'NONE',  ( 11.69610966801475449, -6.874282731906364852, 315.0000000000000000 ) ) ;
#5372 = CARTESIAN_POINT ( 'NONE',  ( 14.67553856548000013, 5.592168771406000438, -314.4150829855000211 ) ) ;
#5373 = FACE_OUTER_BOUND ( 'NONE', #3387, .T. ) ;
#5374 = MANIFOLD_SOLID_BREP ( 'Stock-MAS-686-1', #9511 ) ;
#5375 = CARTESIAN_POINT ( 'NONE',  ( -18.85102544288001170, 0.8044398135754999846, 319.9928079742500131 ) ) ;
#5376 = CARTESIAN_POINT ( 'NONE',  ( -53.50011725782000127, 2.656480000000000175, -412.5186446566000313 ) ) ;
#5377 = PLANE ( 'NONE',  #8441 ) ;
#5378 = VERTEX_POINT ( 'NONE', #7121 ) ;
#5379 = CARTESIAN_POINT ( 'NONE',  ( -14.73022282720999598, 7.961369676960005748, -317.5770954168139610 ) ) ;
#5380 = CARTESIAN_POINT ( 'NONE',  ( -19.95007997204999839, -1.762487863542002486, -317.0792622552969533 ) ) ;
#5381 = MECHANICAL_DESIGN_GEOMETRIC_PRESENTATION_REPRESENTATION (  '', ( #8640 ), #3849 ) ;
#5382 = CLOSED_SHELL ( 'NONE', ( #3351, #8609, #9379, #964, #1287, #6194, #6341, #47, #4694, #819, #1094, #3379, #8631 ) ) ;
#5383 = DIRECTION ( 'NONE',  ( 0.8820010751365675583, 0.000000000000000000, 0.4712473909295827323 ) ) ;
#5384 = CARTESIAN_POINT ( 'NONE',  ( 17.50000000158812696, 0.4607171203178882513, -314.4995147730188592 ) ) ;
#5385 = EDGE_CURVE ( 'NONE', #6619, #661, #5396, .T. ) ;
#5386 = VECTOR ( 'NONE', #4718, 1000.000000000000114 ) ;
#5387 = EDGE_LOOP ( 'NONE', ( #3618, #7032, #3894, #38 ) ) ;
#5388 = CARTESIAN_POINT ( 'NONE',  ( -9.542482902900836450, -2.500000000000000000, -498.6999609700373526 ) ) ;
#5389 = VERTEX_POINT ( 'NONE', #8926 ) ;
#5390 = CYLINDRICAL_SURFACE ( 'NONE', #5005, 14.00000000000000355 ) ;
#5391 = ORIENTED_EDGE ( 'NONE', *, *, #27, .T. ) ;
#5392 = FACE_BOUND ( 'NONE', #8344, .T. ) ;
#5393 = CARTESIAN_POINT ( 'NONE',  ( -17.60320223513998172, -4.128492944088002048, -302.5071922382879279 ) ) ;
#5394 = B_SPLINE_CURVE_WITH_KNOTS ( 'NONE', 3,
 ( #7212, #3120, #5589, #3281, #1515, #4795, #8066, #5639, #8924, #9789, #2427, #5695, #1568, #3554, #10104, #3394, #7632, #8431, #4145, #970, #10056, #8276, #5910, #4256, #7477, #5801, #9203, #1887, #8384, #6784, #6725, #2746, #1837, #5159, #1939, #3340, #5104, #5851, #7527 ),
 .UNSPECIFIED., .F., .F.,
 ( 4, 1, 1, 1, 1, 1, 1, 1, 1, 1, 1, 1, 1, 1, 1, 1, 1, 1, 1, 1, 1, 1, 1, 1, 1, 1, 1, 1, 1, 1, 1, 1, 1, 1, 1, 1, 4 ),
 ( 0.000000000000000000, 0.02777777777778000015, 0.05555555555556000030, 0.08333333333333001192, 0.1111111111111000027, 0.1388888888888999973, 0.1666666666667000196, 0.1944444444444000109, 0.2222222222222000054, 0.2500000000000000000, 0.2777777777777999946, 0.3055555555555999891, 0.3333333333333000081, 0.3611111111111000027, 0.3888888888888999973, 0.4166666666666999919, 0.4444444444444000109, 0.4722222222222000054, 0.5000000000000000000, 0.5277777777777999946, 0.5555555555555999891, 0.5833333333333000637, 0.6111111111111000582, 0.6388888888888999418, 0.6666666666667000474, 0.6944444444444000109, 0.7222222222222000054, 0.7500000000000000000, 0.7777777777777999946, 0.8055555555555999891, 0.8333333333333000637, 0.8611111111111000582, 0.8888888888888999418, 0.9166666666667000474, 0.9444444444444000109, 0.9722222222222000054, 1.000000000000000000 ),
 .UNSPECIFIED. ) ;
#5395 = CARTESIAN_POINT ( 'NONE',  ( -17.01838671672000203, -2.500000000000000000, -497.7560445212000104 ) ) ;
#5396 = CIRCLE ( 'NONE', #775, 15.50000000000000711 ) ;
#5397 = LINE ( 'NONE', #1317, #6840 ) ;
#5398 =( NAMED_UNIT ( * ) PLANE_ANGLE_UNIT ( ) SI_UNIT ( $, .RADIAN. ) );
#5399 = CARTESIAN_POINT ( 'NONE',  ( 18.86301435545000871, -0.4770680115090000228, -302.5071922382879279 ) ) ;
#5400 = CARTESIAN_POINT ( 'NONE',  ( -11.25912153621000300, -10.42419777155999938, 319.5792614743400009 ) ) ;
#5401 = CARTESIAN_POINT ( 'NONE',  ( 17.34500932694999875, -0.6070218422356999932, -314.6383426456000052 ) ) ;
#5402 = CARTESIAN_POINT ( 'NONE',  ( -15.43693218238999876, 4.538485726840999490, 314.6383426456000052 ) ) ;
#5403 = ORIENTED_EDGE ( 'NONE', *, *, #313, .T. ) ;
#5404 = CARTESIAN_POINT ( 'NONE',  ( 4.927840600415999361, 12.12262669806999149, 318.8802828394900644 ) ) ;
#5405 = CARTESIAN_POINT ( 'NONE',  ( -37.45790571718422513, -8.000000000000000000, -422.6951089173222726 ) ) ;
#5406 = ADVANCED_FACE ( 'NONE', ( #10591 ), #4897, .T. ) ;
#5407 = ORIENTED_EDGE ( 'NONE', *, *, #184, .T. ) ;
#5408 = CARTESIAN_POINT ( 'NONE',  ( -15.54870946350325767, -2.500000000000000000, -436.1258788022018393 ) ) ;
#5409 = CARTESIAN_POINT ( 'NONE',  ( 17.40348244433856806, -5.898854237752688690, 315.0000000000000000 ) ) ;
#5410 = CARTESIAN_POINT ( 'NONE',  ( -16.84526280568076118, 1.268064982489031545, 315.0000000000000568 ) ) ;
#5411 = CARTESIAN_POINT ( 'NONE',  ( -20.00000000032979131, -7.322330470066152230, 190.9999999999999432 ) ) ;
#5412 = PRODUCT_DEFINITION_FORMATION_WITH_SPECIFIED_SOURCE ( 'ANY', '', #3726, .NOT_KNOWN. ) ;
#5413 = CARTESIAN_POINT ( 'NONE',  ( -8.647412455283770782, -8.167526177888579042, -315.0000000000000000 ) ) ;
#5414 = CARTESIAN_POINT ( 'NONE',  ( 20.00000000000000355, 25.00000000015544543, 191.0000000000000000 ) ) ;
#5415 = FACE_OUTER_BOUND ( 'NONE', #6240, .T. ) ;
#5416 = DIRECTION ( 'NONE',  ( -0.000000000000000000, 1.000000000000000000, 0.000000000000000000 ) ) ;
#5417 = CARTESIAN_POINT ( 'NONE',  ( 5.334282155825492033, 9.025044196641820449, -314.9999999999999432 ) ) ;
#5418 = CARTESIAN_POINT ( 'NONE',  ( -19.10187173594998811, 2.686732971880998910, 189.9229057364800042 ) ) ;
#5419 = CARTESIAN_POINT ( 'NONE',  ( 17.50000000000002487, 1.995060298004523415E-08, 314.4999385900306947 ) ) ;
#5420 = EDGE_CURVE ( 'NONE', #722, #2333, #6974, .T. ) ;
#5421 = VERTEX_POINT ( 'NONE', #8666 ) ;
#5422 = DIRECTION ( 'NONE',  ( -0.6156614753245245319, 0.000000000000000000, 0.7880107536076076391 ) ) ;
#5423 = AXIS2_PLACEMENT_3D ( 'NONE', #2702, #1999, #7533 ) ;
#5424 = LINE ( 'NONE', #6288, #7853 ) ;
#5425 = CARTESIAN_POINT ( 'NONE',  ( 0.000000000000000000, 0.000000000000000000, 0.000000000000000000 ) ) ;
#5426 = CARTESIAN_POINT ( 'NONE',  ( 16.95014751240671913, -0.8318069206872660271, 315.0000000000000000 ) ) ;
#5427 = CARTESIAN_POINT ( 'NONE',  ( 13.31399140613000043, 6.082710156904999721, -314.8616023057000461 ) ) ;
#5428 = DIRECTION ( 'NONE',  ( 1.881029090955282852E-11, 1.000000000000000000, 2.085935400224071097E-11 ) ) ;
#5429 = CARTESIAN_POINT ( 'NONE',  ( -18.89077695122000122, 0.08689258194099000465, 319.9928079742500131 ) ) ;
#5430 = DIRECTION ( 'NONE',  ( 0.000000000000000000, 0.000000000000000000, -1.000000000000000000 ) ) ;
#5431 = CARTESIAN_POINT ( 'NONE',  ( -1.292800292905149417, -2.607107930518998362, -434.6991840609383644 ) ) ;
#5432 = EDGE_LOOP ( 'NONE', ( #1144, #4151, #8847, #9643 ) ) ;
#5433 = CARTESIAN_POINT ( 'NONE',  ( 4.911540754813998433, 11.70462039183999892, -317.5770954168139610 ) ) ;
#5434 =( BOUNDED_SURFACE ( )  B_SPLINE_SURFACE ( 3, 1, ( 
 ( #436, #8807 ),
 ( #10421, #599 ),
 ( #6391, #9671 ),
 ( #2205, #9618 ),
 ( #3062, #2314 ),
 ( #5525, #1235 ),
 ( #10317, #6228 ) ),
 .UNSPECIFIED., .F., .F., .T. ) 
 B_SPLINE_SURFACE_WITH_KNOTS ( ( 4, 3, 4 ),
 ( 2, 2 ),
 ( 0.006576891565977380054, 0.5000000000000000000, 0.9934231084340230389 ),
 ( 0.000000000000000000, 1.000000000000000000 ),
 .UNSPECIFIED. ) 
 GEOMETRIC_REPRESENTATION_ITEM ( )  RATIONAL_B_SPLINE_SURFACE ( (
 ( 0.9922222087809804414, 0.9922222087809804414),
 ( 0.8003084355045906317, 0.8003084355045906317),
 ( 0.8029010325775971513, 0.8029010325775971513),
 ( 1.000000000000000000, 1.000000000000000000),
 ( 0.8029010325775969292, 0.8029010325775969292),
 ( 0.8003084355045906317, 0.8003084355045906317),
 ( 0.9922222087809811075, 0.9922222087809811075) ) ) 
 REPRESENTATION_ITEM ( '' )  SURFACE ( )  );
#5435 = CARTESIAN_POINT ( 'NONE',  ( -1.581094244357999612, -12.05691037822999867, -317.5770954168139610 ) ) ;
#5436 = CARTESIAN_POINT ( 'NONE',  ( -26.82908671702000802, 2.500000000000000000, -441.1544246730000509 ) ) ;
#5437 = VECTOR ( 'NONE', #7431, 1000.000000000000000 ) ;
#5438 = DIRECTION ( 'NONE',  ( 0.6918631112021742524, 0.000000000000000000, -0.7220286942758217252 ) ) ;
#5439 = VERTEX_POINT ( 'NONE', #812 ) ;
#5440 = CARTESIAN_POINT ( 'NONE',  ( -16.83327205402999738, 5.309787193942999473, 190.0000000000000000 ) ) ;
#5441 = FACE_OUTER_BOUND ( 'NONE', #8141, .T. ) ;
#5442 = ORIENTED_EDGE ( 'NONE', *, *, #9093, .F. ) ;
#5443 = CARTESIAN_POINT ( 'NONE',  ( -12.86685525668169383, 9.583295652123236863, -316.5000000000004547 ) ) ;
#5444 = ORIENTED_EDGE ( 'NONE', *, *, #9625, .T. ) ;
#5445 = CARTESIAN_POINT ( 'NONE',  ( -102.0103468492230547, -2.500000000000000000, -289.6591388711787545 ) ) ;
#5446 = CARTESIAN_POINT ( 'NONE',  ( 19.56025181625999920, 0.5259968871555997794, -302.4229045757450081 ) ) ;
#5447 = CARTESIAN_POINT ( 'NONE',  ( -31.97945899169042505, -2.500000000000000000, -498.3127369250419747 ) ) ;
#5448 = VECTOR ( 'NONE', #7026, 1000.000000000000000 ) ;
#5449 = CARTESIAN_POINT ( 'NONE',  ( -0.2087206657751867478, -7.623098013552001007, -434.4789349137562340 ) ) ;
#5450 = SURFACE_STYLE_FILL_AREA ( #7873 ) ;
#5451 = CARTESIAN_POINT ( 'NONE',  ( 12.29914730983998972, 8.615864166288998760, -302.5071922382879279 ) ) ;
#5452 = CARTESIAN_POINT ( 'NONE',  ( 2.571935587102001985, -12.40832180828999398, 318.8802828394900644 ) ) ;
#5453 = EDGE_LOOP ( 'NONE', ( #5013, #6295, #3594, #2019 ) ) ;
#5454 = CARTESIAN_POINT ( 'NONE',  ( -13.31399140613000043, -6.082710156904999721, -314.8616023057000461 ) ) ;
#5455 = DIRECTION ( 'NONE',  ( 0.6276613564376926080, 0.000000000000000000, -0.7784864941890744516 ) ) ;
#5456 = ORIENTED_EDGE ( 'NONE', *, *, #10227, .F. ) ;
#5457 = LINE ( 'NONE', #1171, #3976 ) ;
#5458 = CARTESIAN_POINT ( 'NONE',  ( -1.725270327277327764, -7.432960991927813232, -434.7202860689826025 ) ) ;
#5459 = CARTESIAN_POINT ( 'NONE',  ( -15.00000000000072120, 0.4945770392355430256, 315.0000000000001705 ) ) ;
#5460 = EDGE_CURVE ( 'NONE', #5868, #2618, #5698, .T. ) ;
#5461 = ORIENTED_EDGE ( 'NONE', *, *, #7790, .T. ) ;
#5462 = CARTESIAN_POINT ( 'NONE',  ( -10.41198510038999991, -7.677033091942000453, 314.8616023057000461 ) ) ;
#5463 = CARTESIAN_POINT ( 'NONE',  ( -36.01445213885307339, -2.500000000000000000, -460.8005622778243264 ) ) ;
#5464 = CYLINDRICAL_SURFACE ( 'NONE', #7765, 5.000000000000006217 ) ;
#5465 = CARTESIAN_POINT ( 'NONE',  ( -15.63927740852997950, -6.344868560643003974, 319.9928079742500131 ) ) ;
#5466 = CARTESIAN_POINT ( 'NONE',  ( -8.377487131979357571, -8.255758461348163380, -315.0000000000000000 ) ) ;
#5467 = CARTESIAN_POINT ( 'NONE',  ( 17.49999999911143433, -5.867334123717693473, 190.0000000000003411 ) ) ;
#5468 = EDGE_CURVE ( 'NONE', #4588, #9045, #64, .T. ) ;
#5469 = EDGE_LOOP ( 'NONE', ( #583, #4865, #3295, #4954 ) ) ;
#5470 = CARTESIAN_POINT ( 'NONE',  ( -10.00000000000000000, -2.500000000000000000, -315.0000000000000000 ) ) ;
#5471 = EDGE_CURVE ( 'NONE', #2720, #4571, #8628, .T. ) ;
#5472 = VECTOR ( 'NONE', #2996, 1000.000000000000000 ) ;
#5473 = CARTESIAN_POINT ( 'NONE',  ( 2.737481088004029228, 9.377302004685557080, -315.0000000000000000 ) ) ;
#5474 = CARTESIAN_POINT ( 'NONE',  ( -20.06806562977000752, -0.4074806926876002322, 190.4207385301700128 ) ) ;
#5475 = CARTESIAN_POINT ( 'NONE',  ( 9.425114110370859777, 8.435515975020026147, 314.4999463140482021 ) ) ;
#5476 = CARTESIAN_POINT ( 'NONE',  ( -100.2082379103963063, -7.500000000000000000, -339.7166298527751565 ) ) ;
#5477 = AXIS2_PLACEMENT_3D ( 'NONE', #4980, #7454, #98 ) ;
#5478 = CARTESIAN_POINT ( 'NONE',  ( -28.01838671672000203, 2.500000000000000000, -497.7560445212000104 ) ) ;
#5479 = APPLICATION_PROTOCOL_DEFINITION ( 'draft international standard', 'automotive_design', 1998, #2761 ) ;
#5480 = CARTESIAN_POINT ( 'NONE',  ( 4.603463306792016319, -9.141632142122212201, 315.0000000000000568 ) ) ;
#5481 = CARTESIAN_POINT ( 'NONE',  ( 14.38384290288000145, 5.252906928686999599, -314.8616023057000461 ) ) ;
#5482 = EDGE_CURVE ( 'NONE', #7772, #2010, #1403, .T. ) ;
#5483 = CARTESIAN_POINT ( 'NONE',  ( -27.92645732311634532, -9.000000000000001776, -417.8271580078818488 ) ) ;
#5484 = CARTESIAN_POINT ( 'NONE',  ( -16.69571944143998365, 6.308604365468005071, 320.0770942683900557 ) ) ;
#5485 = DIRECTION ( 'NONE',  ( 0.000000000000000000, -1.000000000000000000, 0.000000000000000000 ) ) ;
#5486 = CARTESIAN_POINT ( 'NONE',  ( -1.412886213222854792, -2.524971379295001928, -434.5374950603134039 ) ) ;
#5487 = ORIENTED_EDGE ( 'NONE', *, *, #1537, .F. ) ;
#5488 = CARTESIAN_POINT ( 'NONE',  ( -16.93681971163998057, 6.782628217974004059, -317.0792622552969533 ) ) ;
#5489 = VECTOR ( 'NONE', #6536, 1000.000000000000000 ) ;
#5490 = CARTESIAN_POINT ( 'NONE',  ( -18.53690224725999514, -4.739426065905003149, -316.3802825947000201 ) ) ;
#5491 = CARTESIAN_POINT ( 'NONE',  ( -15.67978886374999803, -4.575336738469999887, -315.0000000000000000 ) ) ;
#5492 = AXIS2_PLACEMENT_3D ( 'NONE', #3285, #5055, #3451 ) ;
#5493 = CARTESIAN_POINT ( 'NONE',  ( -17.42734739651273301, 0.9144542625322023000, -314.5039539236788073 ) ) ;
#5494 = ORIENTED_EDGE ( 'NONE', *, *, #10149, .F. ) ;
#5495 = CARTESIAN_POINT ( 'NONE',  ( -16.63787452912266929, -3.035984518719815561, -314.5459997954131950 ) ) ;
#5496 = ORIENTED_EDGE ( 'NONE', *, *, #7702, .F. ) ;
#5497 = CARTESIAN_POINT ( 'NONE',  ( 14.93376631645305075, 8.332910267862528642, -316.5000000000004547 ) ) ;
#5498 = VERTEX_POINT ( 'NONE', #8385 ) ;
#5499 = CARTESIAN_POINT ( 'NONE',  ( -4.934712326437797003, -9.087261561615623151, 315.0000000000000000 ) ) ;
#5500 = CARTESIAN_POINT ( 'NONE',  ( 12.66297984401999166, -9.215363186789998551, -302.4229045757450081 ) ) ;
#5501 = DIRECTION ( 'NONE',  ( 1.000000000000000000, 0.000000000000000000, 0.000000000000000000 ) ) ;
#5502 = CIRCLE ( 'NONE', #878, 11.00000000000000000 ) ;
#5503 = CARTESIAN_POINT ( 'NONE',  ( -18.21470573400001669, 4.474143576597000127, -302.4229045757450081 ) ) ;
#5504 = EDGE_CURVE ( 'NONE', #8504, #6903, #1581, .T. ) ;
#5505 = FACE_OUTER_BOUND ( 'NONE', #6177, .T. ) ;
#5506 = VERTEX_POINT ( 'NONE', #2699 ) ;
#5507 = CARTESIAN_POINT ( 'NONE',  ( 1.409290114754000012, -9.868237606049000021, -314.6383426456000052 ) ) ;
#5508 = B_SPLINE_CURVE_WITH_KNOTS ( 'NONE', 1,
 ( #3117, #707 ),
 .UNSPECIFIED., .F., .F.,
 ( 2, 2 ),
 ( 0.01907785912498588185, 0.8020667992272814129 ),
 .UNSPECIFIED. ) ;
#5509 = CARTESIAN_POINT ( 'NONE',  ( 11.29198477113000010, 9.236539717938999416, -302.5000000000000000 ) ) ;
#5510 = ORIENTED_EDGE ( 'NONE', *, *, #6017, .T. ) ;
#5511 = CARTESIAN_POINT ( 'NONE',  ( 19.54676335584001023, -0.8901129224502002391, 189.9229057364800042 ) ) ;
#5512 = DIRECTION ( 'NONE',  ( 0.000000000000000000, 0.000000000000000000, -1.000000000000000000 ) ) ;
#5513 = FACE_OUTER_BOUND ( 'NONE', #91, .T. ) ;
#5514 =( BOUNDED_SURFACE ( )  B_SPLINE_SURFACE ( 3, 3, ( 
 ( #7670, #409, #4599, #6921, #4396, #3738, #9441, #8520, #9489, #2076, #1163, #8467, #7872, #521, #1114, #6105, #10194, #5340, #2838, #2130, #3793, #10089, #9392, #464, #4543, #2730, #5998, #10299 ),
 ( #9292, #7720, #2027, #1977, #2779, #5194, #4442, #362, #5293, #8566, #4487, #7766, #8133, #10549, #4857, #6463, #922, #771, #8284, #4053, #7382, #7329, #4101, #1370, #16, #6571, #9906, #3242 ),
 ( #9745, #10348, #4907, #3191, #8232, #9541, #2385, #822, #3353, #4155, #7276, #8185, #6519, #5651, #2986, #3291, #9855, #7081, #5759, #5708, #1735, #2494, #869, #6261, #2181, #9048, #8936, #2543 ),
 ( #8994, #6629, #2438, #571, #1683, #71, #7432, #10599, #5449, #4957, #5808, #9102, #5004, #1580, #1633, #8727, #4652, #9801, #7925, #3992, #1790, #5167, #2806, #1030, #9152, #8496, #7642, #2652 ) ),
 .UNSPECIFIED., .F., .F., .T. ) 
 B_SPLINE_SURFACE_WITH_KNOTS ( ( 4, 4 ),
 ( 4, 1, 1, 1, 1, 1, 1, 1, 1, 1, 1, 1, 1, 1, 1, 1, 1, 1, 1, 1, 1, 1, 1, 1, 1, 4 ),
 ( 0.000000000000000000, 1.000000000000000000 ),
 ( 0.07767058905990999185, 0.08939152241064000914, 0.1081359403480000037, 0.1244563457409999935, 0.1388518310880000051, 0.1526992796679999820, 0.1668709527589999908, 0.1819108867230999904, 0.1983140371714000039, 0.2165053751373000046, 0.2367746643099999937, 0.2591785502784000328, 0.2836740072810999824, 0.3102501903660999649, 0.3389525715886999579, 0.3700542176499000413, 0.4038975325576000253, 0.4407462203071000340, 0.4805450085883000155, 0.5231138182776999823, 0.5682755275442999965, 0.6162057510130999338, 0.6675662233626999953, 0.7230529014809999877, 0.7833591819763000563, 0.8073089092479999174 ),
 .UNSPECIFIED. ) 
 GEOMETRIC_REPRESENTATION_ITEM ( )  RATIONAL_B_SPLINE_SURFACE ( (
 ( 1.026133035016000061, 1.026133035016000061, 1.026133035016000061, 1.026133035016000061, 1.026133035016000061, 1.026133035016000061, 1.026133035016000061, 1.026133035016000061, 1.026133035016000061, 1.026133035016000061, 1.026133035016000061, 1.026133035016000061, 1.026133035016000061, 1.026133035016000061, 1.026133035016000061, 1.026133035016000061, 1.026133035016000061, 1.026133035016000061, 1.026133035016000061, 1.026133035016000061, 1.026133035016000061, 1.026133035016000061, 1.026133035016000061, 1.026133035016000061, 1.026133035016000061, 1.026133035016000061, 1.026133035016000061, 1.026133035016000061),
 ( 0.9912889883279000225, 0.9912889883279000225, 0.9912889883279000225, 0.9912889883279000225, 0.9912889883279000225, 0.9912889883279000225, 0.9912889883279000225, 0.9912889883279000225, 0.9912889883279000225, 0.9912889883279000225, 0.9912889883279000225, 0.9912889883279000225, 0.9912889883279000225, 0.9912889883279000225, 0.9912889883279000225, 0.9912889883279000225, 0.9912889883279000225, 0.9912889883279000225, 0.9912889883279000225, 0.9912889883279000225, 0.9912889883279000225, 0.9912889883279000225, 0.9912889883279000225, 0.9912889883279000225, 0.9912889883279000225, 0.9912889883279000225, 0.9912889883279000225, 0.9912889883279000225),
 ( 0.9912889883279000225, 0.9912889883279000225, 0.9912889883279000225, 0.9912889883279000225, 0.9912889883279000225, 0.9912889883279000225, 0.9912889883279000225, 0.9912889883279000225, 0.9912889883279000225, 0.9912889883279000225, 0.9912889883279000225, 0.9912889883279000225, 0.9912889883279000225, 0.9912889883279000225, 0.9912889883279000225, 0.9912889883279000225, 0.9912889883279000225, 0.9912889883279000225, 0.9912889883279000225, 0.9912889883279000225, 0.9912889883279000225, 0.9912889883279000225, 0.9912889883279000225, 0.9912889883279000225, 0.9912889883279000225, 0.9912889883279000225, 0.9912889883279000225, 0.9912889883279000225),
 ( 1.026133035016000061, 1.026133035016000061, 1.026133035016000061, 1.026133035016000061, 1.026133035016000061, 1.026133035016000061, 1.026133035016000061, 1.026133035016000061, 1.026133035016000061, 1.026133035016000061, 1.026133035016000061, 1.026133035016000061, 1.026133035016000061, 1.026133035016000061, 1.026133035016000061, 1.026133035016000061, 1.026133035016000061, 1.026133035016000061, 1.026133035016000061, 1.026133035016000061, 1.026133035016000061, 1.026133035016000061, 1.026133035016000061, 1.026133035016000061, 1.026133035016000061, 1.026133035016000061, 1.026133035016000061, 1.026133035016000061) ) ) 
 REPRESENTATION_ITEM ( '' )  SURFACE ( )  );
#5515 = CARTESIAN_POINT ( 'NONE',  ( -16.78232460783999969, -3.056336161456999712, 314.4150829855000211 ) ) ;
#5516 = CYLINDRICAL_SURFACE ( 'NONE', #7273, 3.500000000000003109 ) ;
#5517 = CARTESIAN_POINT ( 'NONE',  ( 15.68033135863999838, 6.468544937636000469, 320.0000000000000000 ) ) ;
#5518 = CARTESIAN_POINT ( 'NONE',  ( -11.73041118561999951, -8.897639792529000502, 319.9928079742500131 ) ) ;
#5519 = CARTESIAN_POINT ( 'NONE',  ( -16.35767260765813447, -2.566771890333038542, -315.0000000000000568 ) ) ;
#5520 = CYLINDRICAL_SURFACE ( 'NONE', #4889, 12.49999999999998579 ) ;
#5521 = ORIENTED_EDGE ( 'NONE', *, *, #1752, .T. ) ;
#5522 = CARTESIAN_POINT ( 'NONE',  ( -0.6597201369859407860, -2.500000714168999938, -434.1397697187372273 ) ) ;
#5523 = PRODUCT_DEFINITION_SHAPE ( 'NONE', 'NONE',  #10627 ) ;
#5524 = CARTESIAN_POINT ( 'NONE',  ( 2.614541635441999468, 11.98958966642998902, 189.9229057364800042 ) ) ;
#5525 = CARTESIAN_POINT ( 'NONE',  ( -17.49999999911142723, 5.867334123717705907, -302.5000000000003411 ) ) ;
#5526 = CIRCLE ( 'NONE', #7088, 3.500000000000005773 ) ;
#5527 = PRODUCT_RELATED_PRODUCT_CATEGORY ( 'part', '', ( #3726 ) ) ;
#5528 = DIRECTION ( 'NONE',  ( 0.000000000000000000, 1.000000000000000000, 0.000000000000000000 ) ) ;
#5529 = DIRECTION ( 'NONE',  ( 0.000000000000000000, 1.000000000000000000, 0.000000000000000000 ) ) ;
#5530 =( NAMED_UNIT ( * ) SI_UNIT ( $, .STERADIAN. ) SOLID_ANGLE_UNIT ( ) );
#5531 = CARTESIAN_POINT ( 'NONE',  ( -16.84717009645851249, -6.762270094121639374, -303.4999999999996589 ) ) ;
#5532 = CARTESIAN_POINT ( 'NONE',  ( 16.75097866579000083, 2.074182492207000461, -314.8616023057000461 ) ) ;
#5533 = CARTESIAN_POINT ( 'NONE',  ( -30.41084982323499730, -7.500000000000000000, -460.5301199443746327 ) ) ;
#5534 = CARTESIAN_POINT ( 'NONE',  ( -2.538616493050997569, 11.99586634586999523, 320.0770942683900557 ) ) ;
#5535 = CYLINDRICAL_SURFACE ( 'NONE', #6076, 10.00000000000000533 ) ;
#5536 = CARTESIAN_POINT ( 'NONE',  ( -1.940862085953413141, -2.551169835479998316, -434.7454087554588682 ) ) ;
#5537 = ORIENTED_EDGE ( 'NONE', *, *, #8619, .F. ) ;
#5538 = CARTESIAN_POINT ( 'NONE',  ( -15.01674827698000314, 8.369013993811000418, -317.0792622552969533 ) ) ;
#5539 = CARTESIAN_POINT ( 'NONE',  ( 15.95659996325998087, -7.548489772182000124, -316.3802825947000201 ) ) ;
#5540 = AXIS2_PLACEMENT_3D ( 'NONE', #5880, #255, #4123 ) ;
#5541 = ORIENTED_EDGE ( 'NONE', *, *, #3982, .T. ) ;
#5542 = DIRECTION ( 'NONE',  ( 0.000000000000000000, 0.000000000000000000, 1.000000000000000000 ) ) ;
#5543 = CARTESIAN_POINT ( 'NONE',  ( -72.90663470096859555, -2.500000000000000000, -371.7168990827444190 ) ) ;
#5544 = PLANE ( 'NONE',  #1945 ) ;
#5545 = ORIENTED_EDGE ( 'NONE', *, *, #6330, .F. ) ;
#5546 = CARTESIAN_POINT ( 'NONE',  ( -9.017403168880006703, -8.607149246413708710, -314.5455549245388056 ) ) ;
#5547 = AXIS2_PLACEMENT_3D ( 'NONE', #7868, #2879, #8672 ) ;
#5548 = VERTEX_POINT ( 'NONE', #120 ) ;
#5549 = CARTESIAN_POINT ( 'NONE',  ( -13.93637444108895096, 8.981144148067276234, -316.5000000000004547 ) ) ;
#5550 = EDGE_LOOP ( 'NONE', ( #6256, #4029, #4665, #2842 ) ) ;
#5551 = CARTESIAN_POINT ( 'NONE',  ( -13.98386538276810498, -5.376986245914816109, 315.0000000000000568 ) ) ;
#5552 = CARTESIAN_POINT ( 'NONE',  ( 18.87180507196998747, 0.3567823988189002815, -302.5071922382879279 ) ) ;
#5553 = EDGE_CURVE ( 'NONE', #6664, #6471, #7686, .T. ) ;
#5554 = CLOSED_SHELL ( 'NONE', ( #6120, #9252, #3446, #7191, #9502, #3121, #7268, #1485, #3589, #4308, #3189, #3113, #3818, #9892, #7391, #1477, #3669, #6945, #5664, #6727, #3658, #4620, #1535, #5052, #9969, #10611, #1943, #5291, #2575 ) ) ;
#5555 = FACE_OUTER_BOUND ( 'NONE', #9323, .T. ) ;
#5556 = CIRCLE ( 'NONE', #8645, 3.500000000000020428 ) ;
#5557 = CIRCLE ( 'NONE', #4019, 3.500000000000003109 ) ;
#5558 =( NAMED_UNIT ( * ) PLANE_ANGLE_UNIT ( ) SI_UNIT ( $, .RADIAN. ) );
#5559 = CIRCLE ( 'NONE', #9869, 3.499999999999999112 ) ;
#5560 = CARTESIAN_POINT ( 'NONE',  ( -10.36918760129999484, 10.25095399663999451, -302.4229045757450081 ) ) ;
#5561 = CARTESIAN_POINT ( 'NONE',  ( -9.073652982438993320, -11.14186456285000126, 318.8802828394900644 ) ) ;
#5562 = ORIENTED_EDGE ( 'NONE', *, *, #9616, .F. ) ;
#5563 = CARTESIAN_POINT ( 'NONE',  ( -10.41198510038999991, -7.677033091942000453, -314.8616023057000461 ) ) ;
#5564 = CARTESIAN_POINT ( 'NONE',  ( 19.00000000000000000, 0.000000000000000000, 319.9999999999899956 ) ) ;
#5565 = ORIENTED_EDGE ( 'NONE', *, *, #1759, .F. ) ;
#5566 = CARTESIAN_POINT ( 'NONE',  ( -19.55151251130001100, -0.8490756357253000930, 189.9229057364800042 ) ) ;
#5567 = CARTESIAN_POINT ( 'NONE',  ( -3.129133257132351353, 12.36387889853562960, 190.9999999999996589 ) ) ;
#5568 = CARTESIAN_POINT ( 'NONE',  ( -2.000000000000000000, 3.500000000000000000, -409.5000000000000000 ) ) ;
#5569 = VECTOR ( 'NONE', #5738, 1000.000000000000000 ) ;
#5570 = AXIS2_PLACEMENT_3D ( 'NONE', #1320, #366, #6875 ) ;
#5571 = VECTOR ( 'NONE', #519, 1000.000000000000000 ) ;
#5572 = ADVANCED_FACE ( 'NONE', ( #5967 ), #379, .F. ) ;
#5573 = CARTESIAN_POINT ( 'NONE',  ( -16.77099092997999819, -1.279831385791999843, 315.0848619657999734 ) ) ;
#5574 = SURFACE_STYLE_FILL_AREA ( #9661 ) ;
#5575 = CARTESIAN_POINT ( 'NONE',  ( -8.531707904373998730, 10.27069628977000093, 320.0000000000000000 ) ) ;
#5576 = CARTESIAN_POINT ( 'NONE',  ( 5.823281502584001679, -10.83177932830000501, 319.9928079742500131 ) ) ;
#5577 = CARTESIAN_POINT ( 'NONE',  ( -19.99997414083857450, 0.3194320646935535080, 319.0000000000005116 ) ) ;
#5578 = CARTESIAN_POINT ( 'NONE',  ( -14.92114876071706320, -4.178597097557942952, -438.6851340455692139 ) ) ;
#5579 = CARTESIAN_POINT ( 'NONE',  ( -38.33299437316763658, -2.500000000000000000, -461.6435047520546391 ) ) ;
#5580 = VERTEX_POINT ( 'NONE', #10366 ) ;
#5581 = CYLINDRICAL_SURFACE ( 'NONE', #7245, 3.500000000000003109 ) ;
#5582 = CARTESIAN_POINT ( 'NONE',  ( 10.87058130030999159, 10.04705985032000370, 189.9229057364800042 ) ) ;
#5583 = CARTESIAN_POINT ( 'NONE',  ( -1.662076676062295366, -2.666448017039082963, -434.9964371756940409 ) ) ;
#5584 = EDGE_CURVE ( 'NONE', #1376, #9806, #9840, .T. ) ;
#5585 = CARTESIAN_POINT ( 'NONE',  ( -46.74071243416547361, -2.500000000000000000, -414.3237589990478114 ) ) ;
#5586 = CARTESIAN_POINT ( 'NONE',  ( 15.52919946924948569, 3.840693445095582081, 314.9999999999999432 ) ) ;
#5587 = PRODUCT_CONTEXT ( 'NONE', #9006, 'mechanical' ) ;
#5588 = CARTESIAN_POINT ( 'NONE',  ( 6.533799827619672485, -11.82671337997187599, -303.4999999999996589 ) ) ;
#5589 = CARTESIAN_POINT ( 'NONE',  ( -18.86954045039000150, -1.614942466016999978, -302.4999999999529905 ) ) ;
#5590 = DIRECTION ( 'NONE',  ( 0.000000000000000000, 0.000000000000000000, 1.000000000000000000 ) ) ;
#5591 = CARTESIAN_POINT ( 'NONE',  ( -13.67063500649000396, 8.645526204113002322, 320.0770942683900557 ) ) ;
#5592 = CARTESIAN_POINT ( 'NONE',  ( 7.420201433257000545, 2.500000000000000000, -419.8948508258000061 ) ) ;
#5593 = VERTEX_POINT ( 'NONE', #3872 ) ;
#5594 = CARTESIAN_POINT ( 'NONE',  ( -0.7274534428815968568, -2.498120223866999279, -434.1441721281535138 ) ) ;
#5595 = ORIENTED_EDGE ( 'NONE', *, *, #7378, .F. ) ;
#5596 = CARTESIAN_POINT ( 'NONE',  ( -11.58474654271000048, 9.740515853135002899, -317.5770954168139610 ) ) ;
#5597 = DIRECTION ( 'NONE',  ( -0.9997724835175820779, -0.000000000000000000, 0.02133028834981354205 ) ) ;
#5598 = EDGE_CURVE ( 'NONE', #2578, #7772, #6939, .T. ) ;
#5599 = EDGE_LOOP ( 'NONE', ( #2493, #724, #4550, #7826 ) ) ;
#5600 = FACE_OUTER_BOUND ( 'NONE', #5945, .T. ) ;
#5601 = UNCERTAINTY_MEASURE_WITH_UNIT (LENGTH_MEASURE( 1.000000000000000082E-05 ), #2217, 'distance_accuracy_value', 'NONE');
#5602 = DIRECTION ( 'NONE',  ( 0.000000000000000000, 0.000000000000000000, -1.000000000000000000 ) ) ;
#5603 = PLANE ( 'NONE',  #8976 ) ;
#5604 = ORIENTED_EDGE ( 'NONE', *, *, #762, .F. ) ;
#5605 = ADVANCED_FACE ( 'NONE', ( #3755 ), #378, .T. ) ;
#5606 = CARTESIAN_POINT ( 'NONE',  ( 4.393607043691841518, -12.21170385155074989, 319.0000000000003979 ) ) ;
#5607 = ORIENTED_EDGE ( 'NONE', *, *, #1891, .F. ) ;
#5608 = CARTESIAN_POINT ( 'NONE',  ( -50.24071243418999444, 2.500000000000000000, -414.3237589990000629 ) ) ;
#5609 = ORIENTED_EDGE ( 'NONE', *, *, #4921, .F. ) ;
#5610 = CARTESIAN_POINT ( 'NONE',  ( -13.64105609808563457, -5.653588212731087026, 315.0000000000000000 ) ) ;
#5611 = CARTESIAN_POINT ( 'NONE',  ( -19.57075148197997549, 0.3818783754278996523, -302.4229045757450081 ) ) ;
#5612 = ADVANCED_FACE ( 'NONE', ( #2201 ), #6171, .F. ) ;
#5613 = DIRECTION ( 'NONE',  ( 0.1071946444232947937, 0.000000000000000000, -0.9942380540931651245 ) ) ;
#5614 = CARTESIAN_POINT ( 'NONE',  ( -14.98500449093754483, -6.750000000000000000, -438.4247239981262396 ) ) ;
#5615 = CARTESIAN_POINT ( 'NONE',  ( 13.67213454565999875, 8.648884013374997792, -302.4229045757450081 ) ) ;
#5616 = LINE ( 'NONE', #10399, #2060 ) ;
#5617 = ORIENTED_EDGE ( 'NONE', *, *, #373, .T. ) ;
#5618 = CARTESIAN_POINT ( 'NONE',  ( -8.655660348039997842, -8.816209662726999241, -314.4150829855000211 ) ) ;
#5619 = EDGE_CURVE ( 'NONE', #4497, #9535, #5861, .T. ) ;
#5620 = CARTESIAN_POINT ( 'NONE',  ( -5.500000000000000000, -2.500000000000000000, -409.5000000000000568 ) ) ;
#5621 = ORIENTED_EDGE ( 'NONE', *, *, #7840, .F. ) ;
#5622 = CARTESIAN_POINT ( 'NONE',  ( -2.614541635441999468, -11.98958966642998902, 189.9229057364800042 ) ) ;
#5623 = VECTOR ( 'NONE', #3025, 1000.000000000000000 ) ;
#5624 = DIRECTION ( 'NONE',  ( 0.000000000000000000, -1.000000000000000000, 0.000000000000000000 ) ) ;
#5625 = DIRECTION ( 'NONE',  ( -0.9968876850330226080, 0.000000000000000000, 0.07883491250392142546 ) ) ;
#5626 = CARTESIAN_POINT ( 'NONE',  ( -15.71297435277999810, -3.490404421959999670, 315.0848619657999734 ) ) ;
#5627 = CARTESIAN_POINT ( 'NONE',  ( -11.54587391409000041, 9.118162486329000060, 320.0000000000000000 ) ) ;
#5628 = CARTESIAN_POINT ( 'NONE',  ( 0.6117794464027001000, -11.39410369034999704, 319.9928079742500131 ) ) ;
#5629 = PLANE ( 'NONE',  #5709 ) ;
#5630 = CARTESIAN_POINT ( 'NONE',  ( -14.97631232489547948, -3.822155571840307964, -438.4601715196498048 ) ) ;
#5631 = DIRECTION ( 'NONE',  ( 0.000000000000000000, 1.000000000000000000, 0.000000000000000000 ) ) ;
#5632 = EDGE_LOOP ( 'NONE', ( #1257, #6461, #4996, #3563 ) ) ;
#5633 = CARTESIAN_POINT ( 'NONE',  ( -7.006889269069000115, 6.844138725329000472, -285.0000000000000000 ) ) ;
#5634 = CARTESIAN_POINT ( 'NONE',  ( -8.887010007670999912, 10.76703833147000822, 189.9229057364800042 ) ) ;
#5635 = DIRECTION ( 'NONE',  ( 0.7426245373610527167, 0.000000000000000000, -0.6697079934637800713 ) ) ;
#5636 = CARTESIAN_POINT ( 'NONE',  ( -64.74703706731486363, -12.00000000000000000, -381.8372235071344676 ) ) ;
#5637 = DIRECTION ( 'NONE',  ( 0.000000000000000000, 0.000000000000000000, 1.000000000000000000 ) ) ;
#5638 = CARTESIAN_POINT ( 'NONE',  ( -15.67978886374999803, 4.575336738469999887, -315.0000000000000000 ) ) ;
#5639 = CARTESIAN_POINT ( 'NONE',  ( -15.26659686508999947, -6.829480052022000258, -302.5000000000000000 ) ) ;
#5640 = PRESENTATION_STYLE_ASSIGNMENT (( #3342 ) ) ;
#5641 = APPLICATION_CONTEXT ( 'automotive_design' ) ;
#5642 = CARTESIAN_POINT ( 'NONE',  ( 14.08562033053999585, 8.975362299151996126, 319.5792614743400009 ) ) ;
#5643 = FACE_OUTER_BOUND ( 'NONE', #4748, .T. ) ;
#5644 = CARTESIAN_POINT ( 'NONE',  ( -0.5500890142533868543, -2.522638648632998137, -434.2773879517249611 ) ) ;
#5645 = ORIENTED_EDGE ( 'NONE', *, *, #8567, .F. ) ;
#5646 = CARTESIAN_POINT ( 'NONE',  ( 13.88920775975001298, 9.001345760802989204, -316.3802825947000201 ) ) ;
#5647 = DIRECTION ( 'NONE',  ( -4.963222276338128250E-12, 1.000000000000000000, -2.652296088385032042E-12 ) ) ;
#5648 = AXIS2_PLACEMENT_3D ( 'NONE', #3424, #150, #2623 ) ;
#5649 = CIRCLE ( 'NONE', #1021, 0.5000000000000079936 ) ;
#5650 = CARTESIAN_POINT ( 'NONE',  ( 15.63367387165999922, -6.510275065263000371, 320.0000000000000000 ) ) ;
#5651 = CARTESIAN_POINT ( 'NONE',  ( -0.6014669115574718949, -7.469188726525000988, -434.5943147061385616 ) ) ;
#5652 = CARTESIAN_POINT ( 'NONE',  ( -16.11962419174959393, -7.500000000000000000, -430.9361393731155658 ) ) ;
#5653 = CARTESIAN_POINT ( 'NONE',  ( -2.000000000000000000, -9.500000000000000000, -409.5000000000000000 ) ) ;
#5654 = VERTEX_POINT ( 'NONE', #6225 ) ;
#5655 = AXIS2_PLACEMENT_3D ( 'NONE', #6482, #6310, #9596 ) ;
#5656 = CARTESIAN_POINT ( 'NONE',  ( -14.90286285339068151, -5.148601615201680026, -314.5782021036098399 ) ) ;
#5657 = ORIENTED_EDGE ( 'NONE', *, *, #5731, .F. ) ;
#5658 = CARTESIAN_POINT ( 'NONE',  ( -16.88284456999480199, 6.727435487264397551, -316.5000000000004547 ) ) ;
#5659 = ORIENTED_EDGE ( 'NONE', *, *, #2872, .F. ) ;
#5660 = CARTESIAN_POINT ( 'NONE',  ( -11.93437769929943926, -6.745090416342686801, 315.0000000000000568 ) ) ;
#5661 = CARTESIAN_POINT ( 'NONE',  ( 11.71875184657000091, -10.13482718352000944, -303.6197174156509391 ) ) ;
#5662 = DIRECTION ( 'NONE',  ( -0.000000000000000000, 1.000000000000000000, 0.000000000000000000 ) ) ;
#5663 = DIRECTION ( 'NONE',  ( -0.9712267471052612455, 0.000000000000000000, -0.2381566831044910626 ) ) ;
#5664 = ADVANCED_FACE ( 'NONE', ( #7950 ), #1286, .T. ) ;
#5665 = AXIS2_PLACEMENT_3D ( 'NONE', #2087, #5353, #2943 ) ;
#5666 = ORIENTED_EDGE ( 'NONE', *, *, #704, .T. ) ;
#5667 = CARTESIAN_POINT ( 'NONE',  ( 17.77274276690001287, 5.888218767436999457, -302.9207377450070453 ) ) ;
#5668 = CARTESIAN_POINT ( 'NONE',  ( 19.95862339310001943, -0.9382979884530006087, 318.8802828394900644 ) ) ;
#5669 = ORIENTED_EDGE ( 'NONE', *, *, #6063, .F. ) ;
#5670 = CARTESIAN_POINT ( 'NONE',  ( 6.438474686349000997, -8.964777275824999947, -314.8616023057000461 ) ) ;
#5671 = CARTESIAN_POINT ( 'NONE',  ( 18.99987386368999864, 0.5560526133780999691, -302.5000000001010108 ) ) ;
#5672 = ORIENTED_EDGE ( 'NONE', *, *, #7837, .T. ) ;
#5673 = CARTESIAN_POINT ( 'NONE',  ( 16.71231899867997583, -6.291214601299001785, 189.9229057364800042 ) ) ;
#5674 = CARTESIAN_POINT ( 'NONE',  ( -26.31853765676889267, -7.500000000000000888, -432.7407288192795249 ) ) ;
#5675 = CARTESIAN_POINT ( 'NONE',  ( -12.11078853722071180, 6.646648371397081867, -315.0000000000000000 ) ) ;
#5676 = LINE ( 'NONE', #1548, #4989 ) ;
#5677 = EDGE_CURVE ( 'NONE', #7332, #8193, #2619, .T. ) ;
#5678 = CARTESIAN_POINT ( 'NONE',  ( -17.11849373668000140, -0.6181952683021000317, 314.8616023057000461 ) ) ;
#5679 = ADVANCED_FACE ( 'NONE', ( #2044 ), #9085, .T. ) ;
#5680 = CARTESIAN_POINT ( 'NONE',  ( -19.00000000000000000, 0.000000000000000000, 319.9999999999899956 ) ) ;
#5681 = DIRECTION ( 'NONE',  ( 0.9902680687415800209, 0.000000000000000000, 0.1391731009599966873 ) ) ;
#5682 = CARTESIAN_POINT ( 'NONE',  ( 1.327715439883789150, 12.49239253839650843, 319.0000000000005116 ) ) ;
#5683 = CARTESIAN_POINT ( 'NONE',  ( 17.50000000000001776, -8.653793959161173735E-10, 190.0000000000001137 ) ) ;
#5684 = DIRECTION ( 'NONE',  ( -0.000000000000000000, 1.000000000000000000, 0.000000000000000000 ) ) ;
#5685 = ORIENTED_EDGE ( 'NONE', *, *, #2048, .T. ) ;
#5686 = DIRECTION ( 'NONE',  ( 0.000000000000000000, 0.000000000000000000, -1.000000000000000000 ) ) ;
#5687 = ORIENTED_EDGE ( 'NONE', *, *, #6260, .T. ) ;
#5688 = EDGE_CURVE ( 'NONE', #9634, #2247, #10158, .T. ) ;
#5689 = CIRCLE ( 'NONE', #6907, 1.999999999999998224 ) ;
#5690 = EDGE_LOOP ( 'NONE', ( #5877, #5617, #3960, #7645, #7120, #6414, #1754, #5157, #8139 ) ) ;
#5691 = CARTESIAN_POINT ( 'NONE',  ( -14.00000000000000000, -2.500000000000000000, -380.4979246178999688 ) ) ;
#5692 = CARTESIAN_POINT ( 'NONE',  ( 14.44906369208900365, 4.983045831585199537, 315.0000000000000568 ) ) ;
#5693 = APPLICATION_PROTOCOL_DEFINITION ( 'draft international standard', 'automotive_design', 1998, #4546 ) ;
#5694 = PLANE ( 'NONE',  #8739 ) ;
#5695 = CARTESIAN_POINT ( 'NONE',  ( -11.29198477113000010, -9.236539717938999416, -302.5000000000000000 ) ) ;
#5696 = DIRECTION ( 'NONE',  ( 0.000000000000000000, -1.000000000000000000, 0.000000000000000000 ) ) ;
#5697 = CIRCLE ( 'NONE', #8073, 4.000000000000008882 ) ;
#5698 = LINE ( 'NONE', #6250, #3469 ) ;
#5699 = CARTESIAN_POINT ( 'NONE',  ( -18.24388381812998361, 5.273776366776003144, 319.5792614743400009 ) ) ;
#5700 = FILL_AREA_STYLE ('',( #7426 ) ) ;
#5701 = VECTOR ( 'NONE', #533, 1000.000000000000000 ) ;
#5702 = CARTESIAN_POINT ( 'NONE',  ( -7.006889269069000115, 6.844138725329000472, -284.9999999999999432 ) ) ;
#5703 = DIRECTION ( 'NONE',  ( 0.000000000000000000, -1.000000000000000000, 0.000000000000000000 ) ) ;
#5704 = CARTESIAN_POINT ( 'NONE',  ( 19.97262988322000865, -0.5553097472237004117, -316.3802825947000201 ) ) ;
#5705 = DIRECTION ( 'NONE',  ( 0.000000000000000000, 0.000000000000000000, -1.000000000000000000 ) ) ;
#5706 = EDGE_CURVE ( 'NONE', #8252, #2579, #10523, .T. ) ;
#5707 = PLANE ( 'NONE',  #6478 ) ;
#5708 = CARTESIAN_POINT ( 'NONE',  ( -1.030241670742024773, -7.398214992874999396, -434.8184645790310014 ) ) ;
#5709 = AXIS2_PLACEMENT_3D ( 'NONE', #6769, #9934, #1874 ) ;
#5710 = CARTESIAN_POINT ( 'NONE',  ( -0.5928343448393519344, -2.500000206366000288, -434.1985965821343143 ) ) ;
#5711 = CARTESIAN_POINT ( 'NONE',  ( 14.44867893690424232, -4.983401360453106221, -315.0000000000000000 ) ) ;
#5712 = ORIENTED_EDGE ( 'NONE', *, *, #4458, .F. ) ;
#5713 = CARTESIAN_POINT ( 'NONE',  ( 1.822666172895148984, -9.956379168149531722, -314.5031572587576534 ) ) ;
#5714 = ORIENTED_EDGE ( 'NONE', *, *, #6534, .F. ) ;
#5715 = CARTESIAN_POINT ( 'NONE',  ( -72.90663470102438737, -7.500000000000000888, -371.7168990826883714 ) ) ;
#5716 = EDGE_LOOP ( 'NONE', ( #1810, #4794 ) ) ;
#5717 = CARTESIAN_POINT ( 'NONE',  ( 10.51805095810000346, -10.63699911018001210, -303.6197174156509391 ) ) ;
#5718 = CARTESIAN_POINT ( 'NONE',  ( -1.813125098999968543, -7.427867185880000278, -434.7536662776001322 ) ) ;
#5719 = PLANE ( 'NONE',  #3862 ) ;
#5720 = CARTESIAN_POINT ( 'NONE',  ( -3.435942420224999072, 12.40730057411998821, -302.9207377450070453 ) ) ;
#5721 = AXIS2_PLACEMENT_3D ( 'NONE', #2243, #7351, #5512 ) ;
#5722 = FACE_OUTER_BOUND ( 'NONE', #1969, .T. ) ;
#5723 = ORIENTED_EDGE ( 'NONE', *, *, #30, .F. ) ;
#5724 = CYLINDRICAL_SURFACE ( 'NONE', #87, 3.499999999999999556 ) ;
#5725 = CARTESIAN_POINT ( 'NONE',  ( 6.503149100579999953, 10.80808940222000025, -302.5000000000000000 ) ) ;
#5726 = ORIENTED_EDGE ( 'NONE', *, *, #2896, .T. ) ;
#5727 = CARTESIAN_POINT ( 'NONE',  ( -12.07524870805000639, -10.05998438363999981, 190.4207385301700128 ) ) ;
#5728 = CARTESIAN_POINT ( 'NONE',  ( 13.94567317170587195, 5.407789506212603570, -315.0000000000000000 ) ) ;
#5729 = DIRECTION ( 'NONE',  ( 0.1071946444232959594, 0.000000000000000000, -0.9942380540931649024 ) ) ;
#5730 = AXIS2_PLACEMENT_3D ( 'NONE', #5912, #7634, #5852 ) ;
#5731 = EDGE_CURVE ( 'NONE', #8720, #1105, #297, .T. ) ;
#5732 = CARTESIAN_POINT ( 'NONE',  ( 15.10708484062000068, -4.236041382665999500, 315.0848619657999734 ) ) ;
#5733 =( NAMED_UNIT ( * ) SI_UNIT ( $, .STERADIAN. ) SOLID_ANGLE_UNIT ( ) );
#5734 = CARTESIAN_POINT ( 'NONE',  ( -43.24071243418999444, 2.500000000000000000, -414.3237589990000629 ) ) ;
#5735 = CARTESIAN_POINT ( 'NONE',  ( 13.67063500649000396, -8.645526204113002322, 320.0770942683900557 ) ) ;
#5736 = DIRECTION ( 'NONE',  ( -0.2381566831044910626, 0.000000000000000000, 0.9712267471052612455 ) ) ;
#5737 = CARTESIAN_POINT ( 'NONE',  ( -7.927914882803703378, 11.48831374418035089, -303.4999999999990905 ) ) ;
#5738 = DIRECTION ( 'NONE',  ( 0.000000000000000000, -1.000000000000000000, 0.000000000000000000 ) ) ;
#5739 = VERTEX_POINT ( 'NONE', #7149 ) ;
#5740 = CARTESIAN_POINT ( 'NONE',  ( -20.00000000435073133, 7.322330466772325686, -303.5000000000000000 ) ) ;
#5741 = CIRCLE ( 'NONE', #6247, 2.000000000000007550 ) ;
#5742 = VECTOR ( 'NONE', #63, 999.9999999999998863 ) ;
#5743 = VERTEX_POINT ( 'NONE', #3277 ) ;
#5744 = EDGE_CURVE ( 'NONE', #5251, #10001, #9615, .T. ) ;
#5745 = EDGE_CURVE ( 'NONE', #8113, #4172, #6554, .T. ) ;
#5746 = CARTESIAN_POINT ( 'NONE',  ( -2.000000000000000000, 3.500000000000000000, -409.5000000000000000 ) ) ;
#5747 = CARTESIAN_POINT ( 'NONE',  ( 16.45391189178886293, 2.370722300009959760, 315.0000000000001705 ) ) ;
#5748 = DIRECTION ( 'NONE',  ( 0.000000000000000000, -1.000000000000000000, 0.000000000000000000 ) ) ;
#5749 = CARTESIAN_POINT ( 'NONE',  ( 16.78232460783999969, 3.056336161456999712, -314.4150829855000211 ) ) ;
#5750 = DIRECTION ( 'NONE',  ( -0.9921831154218024862, 0.000000000000000000, -0.1247904863035890766 ) ) ;
#5751 = DIRECTION ( 'NONE',  ( -0.1071946444232964035, 0.000000000000000000, 0.9942380540931649024 ) ) ;
#5752 = EDGE_CURVE ( 'NONE', #8575, #5439, #6731, .T. ) ;
#5753 = CARTESIAN_POINT ( 'NONE',  ( -14.90548258804913928, -5.754348600474655129, -438.7490222628617857 ) ) ;
#5754 = CARTESIAN_POINT ( 'NONE',  ( 14.79012398733999767, 1.483731117707002278, 315.0000000000001705 ) ) ;
#5755 = ORIENTED_EDGE ( 'NONE', *, *, #7155, .F. ) ;
#5756 = CARTESIAN_POINT ( 'NONE',  ( 20.05669107747999291, -0.5612988332226998001, -317.0792622552969533 ) ) ;
#5757 = CARTESIAN_POINT ( 'NONE',  ( -14.00000000000000000, -2.500000000000000000, -380.4979246178999688 ) ) ;
#5758 = CARTESIAN_POINT ( 'NONE',  ( -98.44423576012317767, -7.500000000000000000, -338.7741350709160315 ) ) ;
#5759 = CARTESIAN_POINT ( 'NONE',  ( -0.9445117102953933808, -7.411175710731001232, -434.7797131905516039 ) ) ;
#5760 = DIRECTION ( 'NONE',  ( 0.000000000000000000, 0.000000000000000000, -1.000000000000000000 ) ) ;
#5761 = CARTESIAN_POINT ( 'NONE',  ( 4.934865307815709201, -9.087242801873950171, -315.0000000000000568 ) ) ;
#5762 = ORIENTED_EDGE ( 'NONE', *, *, #10192, .F. ) ;
#5763 = MECHANICAL_DESIGN_GEOMETRIC_PRESENTATION_REPRESENTATION (  '', ( #8171 ), #4739 ) ;
#5764 = CARTESIAN_POINT ( 'NONE',  ( -8.037373804805000077, 9.179324345868998591, -315.0000000000001137 ) ) ;
#5765 = ORIENTED_EDGE ( 'NONE', *, *, #7000, .F. ) ;
#5766 = CARTESIAN_POINT ( 'NONE',  ( 19.00000000000000000, 0.000000000000000000, -317.4999999998989892 ) ) ;
#5767 = ORIENTED_EDGE ( 'NONE', *, *, #1774, .T. ) ;
#5768 = CARTESIAN_POINT ( 'NONE',  ( 10.54839116401999988, -10.71567991178000057, -302.9207377450070453 ) ) ;
#5769 = CARTESIAN_POINT ( 'NONE',  ( 17.62591998684001027, -4.093640041088997705, -317.4928077629770087 ) ) ;
#5770 = DIRECTION ( 'NONE',  ( -0.000000000000000000, 1.000000000000000000, 0.000000000000000000 ) ) ;
#5771 = CARTESIAN_POINT ( 'NONE',  ( 3.692777996438003196, 12.29248881612998190, -303.6197174156520759 ) ) ;
#5772 = CARTESIAN_POINT ( 'NONE',  ( -17.05557420093911958, -2.295407597284876644, 314.4999494796127806 ) ) ;
#5773 = EDGE_LOOP ( 'NONE', ( #8949, #1432 ) ) ;
#5774 = DIRECTION ( 'NONE',  ( 0.000000000000000000, 1.000000000000000000, 0.000000000000000000 ) ) ;
#5775 = DIRECTION ( 'NONE',  ( -0.1071946444232954182, 0.000000000000000000, 0.9942380540931651245 ) ) ;
#5776 = ORIENTED_EDGE ( 'NONE', *, *, #5233, .T. ) ;
#5777 = CARTESIAN_POINT ( 'NONE',  ( 20.05687582562997662, 0.5621360437329007143, 190.4207385301700128 ) ) ;
#5778 = CARTESIAN_POINT ( 'NONE',  ( 0.000000000000000000, -10.54711710274999881, -314.4944826805095772 ) ) ;
#5779 = DIRECTION ( 'NONE',  ( -0.000000000000000000, 1.000000000000000000, 0.000000000000000000 ) ) ;
#5780 = FACE_OUTER_BOUND ( 'NONE', #1827, .T. ) ;
#5781 =( REPRESENTATION_RELATIONSHIP ('NONE','NONE', #8468, #7381 ) REPRESENTATION_RELATIONSHIP_WITH_TRANSFORMATION ( #8273 )SHAPE_REPRESENTATION_RELATIONSHIP( ) );
#5782 = CARTESIAN_POINT ( 'NONE',  ( 16.90798586812000082, 0.2930809059028999797, 315.0848619657999734 ) ) ;
#5783 = CARTESIAN_POINT ( 'NONE',  ( -2.000000000003786749, -9.000000000000001776, -409.4999999999758415 ) ) ;
#5784 = CARTESIAN_POINT ( 'NONE',  ( -1.310287062331999319, -12.07175205226999815, 320.0770942683900557 ) ) ;
#5785 = AXIS2_PLACEMENT_3D ( 'NONE', #8808, #10474, #4790 ) ;
#5786 = DIRECTION ( 'NONE',  ( 0.000000000000000000, 1.000000000000000000, 0.000000000000000000 ) ) ;
#5787 =( NAMED_UNIT ( * ) PLANE_ANGLE_UNIT ( ) SI_UNIT ( $, .RADIAN. ) );
#5788 = CARTESIAN_POINT ( 'NONE',  ( 11.89238025184999792, 6.701939844102000166, 315.0848619657999734 ) ) ;
#5789 = ORIENTED_EDGE ( 'NONE', *, *, #568, .F. ) ;
#5790 = CARTESIAN_POINT ( 'NONE',  ( -0.7126779659677977552, -12.51265294199207823, 190.9999999999995737 ) ) ;
#5791 = ORIENTED_EDGE ( 'NONE', *, *, #4570, .T. ) ;
#5792 = ORIENTED_EDGE ( 'NONE', *, *, #1203, .F. ) ;
#5793 = EDGE_CURVE ( 'NONE', #8235, #9192, #9818, .T. ) ;
#5794 = AXIS2_PLACEMENT_3D ( 'NONE', #1344, #2261, #7154 ) ;
#5795 = B_SPLINE_CURVE_WITH_KNOTS ( 'NONE', 3,
 ( #6505, #1565, #8115, #2477 ),
 .UNSPECIFIED., .F., .F.,
 ( 4, 4 ),
 ( 0.000000000000000000, 1.000000000000000000 ),
 .UNSPECIFIED. ) ;
#5796 = CARTESIAN_POINT ( 'NONE',  ( -6.058905833985400946, -2.720859597169000388, -436.0408773327500285 ) ) ;
#5797 = CARTESIAN_POINT ( 'NONE',  ( 8.673721998911229747, 8.158754989085133857, 315.0000000000000568 ) ) ;
#5798 = CARTESIAN_POINT ( 'NONE',  ( 13.57573464316000056, -3.225916527208000151, -285.0000000000000000 ) ) ;
#5799 = ORIENTED_EDGE ( 'NONE', *, *, #1869, .T. ) ;
#5800 = EDGE_CURVE ( 'NONE', #4863, #2810, #7923, .T. ) ;
#5801 = CARTESIAN_POINT ( 'NONE',  ( 8.922355960362999383, -10.14988298126000110, -302.5000000000000000 ) ) ;
#5802 = CARTESIAN_POINT ( 'NONE',  ( 19.00000000000000000, 0.000000000000000000, 190.0000000000100044 ) ) ;
#5803 = CARTESIAN_POINT ( 'NONE',  ( -99.26574312853713877, -2.500000000000000000, -341.4806320030483562 ) ) ;
#5804 = CARTESIAN_POINT ( 'NONE',  ( -0.1979899810951909478, -2.341947051001003199, -433.8401545479024435 ) ) ;
#5805 = ORIENTED_EDGE ( 'NONE', *, *, #9172, .F. ) ;
#5806 = CARTESIAN_POINT ( 'NONE',  ( -8.092749801746995431, 11.43508185634000007, -316.3802825947000201 ) ) ;
#5807 = CARTESIAN_POINT ( 'NONE',  ( 6.864438614955176376, -4.432289485863268652, -525.3966049790363968 ) ) ;
#5808 = CARTESIAN_POINT ( 'NONE',  ( -0.2960734841582018384, -7.598655014342003078, -434.5913138198718570 ) ) ;
#5809 = DIRECTION ( 'NONE',  ( -0.8820010751365653379, 0.000000000000000000, -0.4712473909295871732 ) ) ;
#5810 = CARTESIAN_POINT ( 'NONE',  ( 12.45686666771074336, -6.446195019498007106, -315.0000000000000568 ) ) ;
#5811 = VERTEX_POINT ( 'NONE', #6387 ) ;
#5812 = CARTESIAN_POINT ( 'NONE',  ( 17.19853431800999743, 2.231396706187000145, -314.4963898845653603 ) ) ;
#5813 = ORIENTED_EDGE ( 'NONE', *, *, #8719, .F. ) ;
#5814 = CARTESIAN_POINT ( 'NONE',  ( -2.000000000000000000, 2.500000000000000000, -409.5000000000000568 ) ) ;
#5815 = EDGE_LOOP ( 'NONE', ( #2285, #1437, #1903, #9448 ) ) ;
#5816 = CARTESIAN_POINT ( 'NONE',  ( 19.95943119690998557, -1.720147047185998757, -302.9207377450070453 ) ) ;
#5817 = VECTOR ( 'NONE', #1736, 1000.000000000000000 ) ;
#5818 = CIRCLE ( 'NONE', #3761, 0.5000000000000004441 ) ;
#5819 = CARTESIAN_POINT ( 'NONE',  ( 1.983867121666000877, -11.33269556189999960, -317.4928077629770087 ) ) ;
#5820 = EDGE_CURVE ( 'NONE', #9461, #3582, #2944, .T. ) ;
#5821 = CARTESIAN_POINT ( 'NONE',  ( -5.262172113226215586, -8.000000000000000000, -337.7350057056290211 ) ) ;
#5822 =( LENGTH_UNIT ( ) NAMED_UNIT ( * ) SI_UNIT ( .MILLI., .METRE. ) );
#5823 = CIRCLE ( 'NONE', #4130, 999.9999999999997726 ) ;
#5824 = CARTESIAN_POINT ( 'NONE',  ( -3.672986306062375750, -7.316704338766061078, -435.3862664917431857 ) ) ;
#5825 = CARTESIAN_POINT ( 'NONE',  ( -14.91230748276000817, -5.270530864637949620, 314.4999479601418102 ) ) ;
#5826 = EDGE_LOOP ( 'NONE', ( #4193, #4534 ) ) ;
#5827 = CARTESIAN_POINT ( 'NONE',  ( -16.92248268936999978, -0.04189409840124999618, -315.0848619657999734 ) ) ;
#5828 = CARTESIAN_POINT ( 'NONE',  ( -4.912752152484999968, 11.11695209346000013, -302.5000000000000000 ) ) ;
#5829 = EDGE_LOOP ( 'NONE', ( #10583, #2006 ) ) ;
#5830 = CARTESIAN_POINT ( 'NONE',  ( -16.39938580555998726, -7.272241081627004000, 190.4207385301700128 ) ) ;
#5831 = CARTESIAN_POINT ( 'NONE',  ( -3.339933055294988851, -8.000000000000000000, -397.0720243238112630 ) ) ;
#5832 = DIRECTION ( 'NONE',  ( 0.6276613564376841703, 0.000000000000000000, -0.7784864941890811130 ) ) ;
#5833 = CARTESIAN_POINT ( 'NONE',  ( -9.036610176479998202, 11.24204914511999398, 190.4207385301700128 ) ) ;
#5834 = ADVANCED_BREP_SHAPE_REPRESENTATION ( '', ( #8937, #2817 ), #7989 ) ;
#5835 = EDGE_CURVE ( 'NONE', #1301, #4961, #3170, .T. ) ;
#5836 = CARTESIAN_POINT ( 'NONE',  ( 14.72449281369000040, -5.549439731021000632, 314.4150829855000211 ) ) ;
#5837 = FILL_AREA_STYLE ('',( #898 ) ) ;
#5838 = LINE ( 'NONE', #9129, #5193 ) ;
#5839 = CARTESIAN_POINT ( 'NONE',  ( -13.82465948680000878, -8.551125454139995696, 320.0770942683900557 ) ) ;
#5840 = DIRECTION ( 'NONE',  ( 0.5828070674935411644, 0.000000000000000000, 0.8126105599114369360 ) ) ;
#5841 = CARTESIAN_POINT ( 'NONE',  ( -13.36185104352900055, -9.000000000000001776, -400.1641368440791098 ) ) ;
#5842 = CARTESIAN_POINT ( 'NONE',  ( 3.932702496464000497, 9.868769537474999964, 314.4150829855000211 ) ) ;
#5843 = ORIENTED_EDGE ( 'NONE', *, *, #6034, .F. ) ;
#5844 = CARTESIAN_POINT ( 'NONE',  ( -4.467179684046219457, -12.20122392890712781, 190.9999999999995737 ) ) ;
#5845 = ORIENTED_EDGE ( 'NONE', *, *, #7520, .T. ) ;
#5846 = CARTESIAN_POINT ( 'NONE',  ( -13.10769452645968691, -4.328281264598399680, -438.3867334686859749 ) ) ;
#5847 = CARTESIAN_POINT ( 'NONE',  ( -8.636532331090950976, 8.171139803988637595, 315.0000000000000568 ) ) ;
#5848 = EDGE_CURVE ( 'NONE', #7332, #3634, #9779, .T. ) ;
#5849 = DIRECTION ( 'NONE',  ( -0.2728306852451987119, 0.000000000000000000, -0.9620620651437387094 ) ) ;
#5850 = ORIENTED_EDGE ( 'NONE', *, *, #2410, .T. ) ;
#5851 = CARTESIAN_POINT ( 'NONE',  ( 18.99984306468000028, -0.5551939808346000316, -302.5000000001010108 ) ) ;
#5852 = DIRECTION ( 'NONE',  ( 0.000000000000000000, -1.000000000000000000, 0.000000000000000000 ) ) ;
#5853 = CARTESIAN_POINT ( 'NONE',  ( -12.01210725212448338, -6.943331886975998124, -437.6899295328262838 ) ) ;
#5854 = CARTESIAN_POINT ( 'NONE',  ( 12.89381010047549303, -6.798165292128601322, 314.4999421354863784 ) ) ;
#5855 = DIRECTION ( 'NONE',  ( -0.3420201433256988555, 0.000000000000000000, 0.9396926207858975477 ) ) ;
#5856 = CARTESIAN_POINT ( 'NONE',  ( -17.50000000000000000, 0.000000000000000000, -315.0000000000000000 ) ) ;
#5857 = CARTESIAN_POINT ( 'NONE',  ( -10.59417419979999586, 10.60664446758999446, -316.3802825947000201 ) ) ;
#5858 = CARTESIAN_POINT ( 'NONE',  ( -51.90260568677000208, -7.500000000000000888, -351.6213581552000278 ) ) ;
#5859 =( BOUNDED_CURVE ( )  B_SPLINE_CURVE ( 3, ( #6279, #8801, #1443, #2850, #6118, #7409, #746, #8911, #1612, #8163, #10578, #9775, #800, #6440, #6383, #644, #8105, #6550, #3324, #4833, #9664, #3969, #2306, #5682, #9024, #4885, #3272, #3221, #9885, #8970, #1660, #9077, #10467, #4080, #10519, #7357, #4026, #1501, #2521, #7197, #4935, #6497, #3887, #8859, #9830, #849, #5577, #4783 ),
 .UNSPECIFIED., .F., .F. ) 
 B_SPLINE_CURVE_WITH_KNOTS ( ( 4, 1, 1, 1, 1, 1, 1, 1, 1, 1, 1, 1, 1, 1, 1, 1, 1, 1, 1, 1, 1, 1, 1, 1, 1, 1, 1, 1, 1, 1, 1, 1, 1, 1, 1, 1, 1, 1, 1, 1, 1, 1, 1, 1, 1, 4 ),
 ( 0.000000000000000000, 0.01696016684112893608, 0.03526043942249617452, 0.05280277254187633329, 0.06993090526874494450, 0.08694163804313655153, 0.1040119350351718791, 0.1210139405588612077, 0.1379792171159073266, 0.1553986424958141432, 0.1736039501722523581, 0.1924119339504005155, 0.2116998327295476212, 0.2316504953696777447, 0.2523434511079294396, 0.2735071578860148178, 0.2951461022590913807, 0.3179819391660331784, 0.3428270683969385502, 0.3704763703089109517, 0.4013842106079446026, 0.4356267894623514492, 0.4731822280981956563, 0.5126799690798770071, 0.5516183454030081368, 0.5879427231221452388, 0.6209690717414464434, 0.6502633940987107009, 0.6759717312850140880, 0.6991685419836423110, 0.7210175260783883155, 0.7426211155567139510, 0.7640811388048154296, 0.7847659435495429880, 0.8046277674085309251, 0.8239473966552023354, 0.8426767883169220541, 0.8606205966378887018, 0.8779797588928680563, 0.8951189492511467671, 0.9121717320952801300, 0.9291919606104407370, 0.9463734364297033963, 0.9639783248497096890, 0.9823161612921426089, 1.000000000000000000 ),
 .UNSPECIFIED. ) 
 CURVE ( )  GEOMETRIC_REPRESENTATION_ITEM ( )  RATIONAL_B_SPLINE_CURVE ( ( 1.171573005652621013, 1.171573005652621235, 1.171573005652621235, 1.171573005652621235, 1.171573005652621235, 1.171573005652621235, 1.171573005652621235, 1.171573005652621235, 1.171573005652621235, 1.171573005652621235, 1.171573005652621235, 1.171573005652621235, 1.171573005652621235, 1.171573005652621235, 1.171573005652621235, 1.171573005652621235, 1.171573005652621235, 1.171573005652621235, 1.171573005652621235, 1.171573005652621235, 1.171573005652621235, 1.171573005652621235, 1.171573005652621235, 1.171573005652621235, 1.171573005652621235, 1.171573005652621235, 1.171573005652621235, 1.171573005652621235, 1.171573005652621235, 1.171573005652621235, 1.171573005652621235, 1.171573005652621235, 1.171573005652621235, 1.171573005652621235, 1.171573005652621235, 1.171573005652621235, 1.171573005652621235, 1.171573005652621235, 1.171573005652621235, 1.171573005652621235, 1.171573005652621235, 1.171573005652621235, 1.171573005652621235, 1.171573005652621235, 1.171573005652621235, 1.171573005652621235, 1.171573005652621235, 1.171573005652621235 ) ) 
 REPRESENTATION_ITEM ( '' )  );
#5860 = CARTESIAN_POINT ( 'NONE',  ( 8.142442032185543965, -5.722112424457679758, -525.7457260455852293 ) ) ;
#5861 = CIRCLE ( 'NONE', #8781, 3.500000000000006217 ) ;
#5862 = CARTESIAN_POINT ( 'NONE',  ( -19.68871134463705985, -9.500000000000001776, -416.4361005590961327 ) ) ;
#5863 = CARTESIAN_POINT ( 'NONE',  ( 4.669917308725584526, -9.131001784561973977, -315.0000000000000000 ) ) ;
#5864 = VERTEX_POINT ( 'NONE', #4888 ) ;
#5865 = CARTESIAN_POINT ( 'NONE',  ( -17.50000000000125056, -1.380497925828168986E-12, -315.0000000000001705 ) ) ;
#5866 = ORIENTED_EDGE ( 'NONE', *, *, #10161, .F. ) ;
#5867 = DIRECTION ( 'NONE',  ( 0.1071946444232958900, 0.000000000000000000, -0.9942380540931649024 ) ) ;
#5868 = VERTEX_POINT ( 'NONE', #9668 ) ;
#5869 = CARTESIAN_POINT ( 'NONE',  ( -13.88537659940002023, -9.003549035645995957, -303.6197174156509391 ) ) ;
#5870 = B_SPLINE_CURVE_WITH_KNOTS ( 'NONE', 3,
 ( #3727, #9529, #1412, #5491, #3776, #10283, #8770, #7807, #1357, #4639, #5280, #2922, #3673 ),
 .UNSPECIFIED., .F., .F.,
 ( 4, 1, 1, 1, 1, 1, 1, 1, 1, 1, 4 ),
 ( 0.000000000000000000, 0.08333333333333001192, 0.1666666666667000196, 0.2500000000000000000, 0.3333333333333000081, 0.5000000000000000000, 0.6666666666667000474, 0.7500000000000000000, 0.8333333333333000637, 0.9166666666667000474, 1.000000000000000000 ),
 .UNSPECIFIED. ) ;
#5871 = ADVANCED_FACE ( 'NONE', ( #2311 ), #5581, .T. ) ;
#5872 = CARTESIAN_POINT ( 'NONE',  ( -18.90056365643000547, -0.3167749459464000994, -317.4928077629770087 ) ) ;
#5873 = CARTESIAN_POINT ( 'NONE',  ( -16.76545246634000108, 2.037063237379999947, -314.8616023057000461 ) ) ;
#5874 = DIRECTION ( 'NONE',  ( 0.000000000000000000, 0.000000000000000000, 1.000000000000000000 ) ) ;
#5875 = CARTESIAN_POINT ( 'NONE',  ( 19.97256092624000701, -0.5562539513971997973, -303.6197174156509391 ) ) ;
#5876 = CARTESIAN_POINT ( 'NONE',  ( -17.49999996772987743, -5.857864456328762515, 314.9999999999999432 ) ) ;
#5877 = ORIENTED_EDGE ( 'NONE', *, *, #2729, .F. ) ;
#5878 = CARTESIAN_POINT ( 'NONE',  ( -0.6596894340221253206, -7.499999891561000886, -434.1397621899948263 ) ) ;
#5879 = EDGE_CURVE ( 'NONE', #3758, #6759, #5172, .T. ) ;
#5880 = CARTESIAN_POINT ( 'NONE',  ( -1.873948611767810357, -2.500000000000000000, -349.2478646809746579 ) ) ;
#5881 = ORIENTED_EDGE ( 'NONE', *, *, #5677, .T. ) ;
#5882 = CARTESIAN_POINT ( 'NONE',  ( 17.06589079541999965, -6.642208448352997507, 190.4207385301700128 ) ) ;
#5883 = CARTESIAN_POINT ( 'NONE',  ( 15.67978886374999803, -4.575336738469999887, -315.0000000000001137 ) ) ;
#5884 = CARTESIAN_POINT ( 'NONE',  ( 16.35767260765813447, 2.566771890333039874, -315.0000000000000000 ) ) ;
#5885 = ADVANCED_FACE ( 'NONE', ( #8109 ), #5958, .F. ) ;
#5886 = DIRECTION ( 'NONE',  ( 0.000000000000000000, -1.000000000000000000, 0.000000000000000000 ) ) ;
#5887 = CARTESIAN_POINT ( 'NONE',  ( 8.858368459239001069, 11.29793033041000250, 190.4207385301700128 ) ) ;
#5888 = VECTOR ( 'NONE', #999, 1000.000000000000000 ) ;
#5889 = CARTESIAN_POINT ( 'NONE',  ( 14.57772014836000096, -5.380605385836000565, 314.6383426456000052 ) ) ;
#5890 = PRESENTATION_STYLE_ASSIGNMENT (( #2626 ) ) ;
#5891 = FACE_OUTER_BOUND ( 'NONE', #34, .T. ) ;
#5892 = CARTESIAN_POINT ( 'NONE',  ( 12.76583521038999613, -9.157751700393998107, 320.0770942683900557 ) ) ;
#5893 = DIRECTION ( 'NONE',  ( 0.000000000000000000, -1.000000000000000000, 0.000000000000000000 ) ) ;
#5894 = CARTESIAN_POINT ( 'NONE',  ( 0.1638132020714604398, 12.51773231663031716, -303.4999999999990905 ) ) ;
#5895 = CARTESIAN_POINT ( 'NONE',  ( 8.655660348039997842, 8.816209662726999241, 314.4150829855000211 ) ) ;
#5896 = EDGE_LOOP ( 'NONE', ( #1700, #2391 ) ) ;
#5897 = CARTESIAN_POINT ( 'NONE',  ( 6.404755722164563458, -11.85477825286778319, 190.9999999999995737 ) ) ;
#5898 = CARTESIAN_POINT ( 'NONE',  ( 19.58476356052999279, 2.818858455686998887, 319.5792614743400009 ) ) ;
#5899 = ORIENTED_EDGE ( 'NONE', *, *, #8111, .F. ) ;
#5900 = EDGE_CURVE ( 'NONE', #8899, #9423, #9938, .T. ) ;
#5901 = CIRCLE ( 'NONE', #408, 0.5000000000000083267 ) ;
#5902 = CIRCLE ( 'NONE', #1266, 13.99999999999999645 ) ;
#5903 = AXIS2_PLACEMENT_3D ( 'NONE', #2649, #232, #1894 ) ;
#5904 = CARTESIAN_POINT ( 'NONE',  ( -10.10898320382307602, -3.650023814309998116, -437.2731589972925121 ) ) ;
#5905 = CARTESIAN_POINT ( 'NONE',  ( -1.962900534989000745, 9.435972684515721909, 314.9999999999999432 ) ) ;
#5906 = VECTOR ( 'NONE', #747, 1000.000000000000000 ) ;
#5907 = CARTESIAN_POINT ( 'NONE',  ( -15.00000000000325784, 8.632726818195413123E-17, 315.0000000000001705 ) ) ;
#5908 = VECTOR ( 'NONE', #194, 1000.000000000000000 ) ;
#5909 = VERTEX_POINT ( 'NONE', #1828 ) ;
#5910 = CARTESIAN_POINT ( 'NONE',  ( 4.912752152484999968, -11.11695209346000013, -302.5000000000000000 ) ) ;
#5911 = VECTOR ( 'NONE', #2983, 1000.000000000000114 ) ;
#5912 = CARTESIAN_POINT ( 'NONE',  ( -37.57635160138833896, -9.000000000000001776, -403.2777420460153053 ) ) ;
#5913 = CARTESIAN_POINT ( 'NONE',  ( 5.950428891765999317, 10.92854977363000124, 190.0000000000000000 ) ) ;
#5914 = DIRECTION ( 'NONE',  ( -0.1247904863035888268, 0.000000000000000000, 0.9921831154218024862 ) ) ;
#5915 = VERTEX_POINT ( 'NONE', #9248 ) ;
#5916 = DIRECTION ( 'NONE',  ( 0.000000000000000000, 0.000000000000000000, -1.000000000000000000 ) ) ;
#5917 = AXIS2_PLACEMENT_3D ( 'NONE', #6042, #1915, #3681 ) ;
#5918 = COLOUR_RGB ( '', 0.72549020, 0.75294118, 0.79215686) ;
#5919 = FACE_BOUND ( 'NONE', #3418, .T. ) ;
#5920 = CARTESIAN_POINT ( 'NONE',  ( 8.650620448811780605, -5.791189843283389926, -525.6331420297578916 ) ) ;
#5921 = UNCERTAINTY_MEASURE_WITH_UNIT (LENGTH_MEASURE( 1.000000000000000082E-05 ), #9665, 'distance_accuracy_value', 'NONE');
#5922 = CARTESIAN_POINT ( 'NONE',  ( 10.00000000000000000, 2.500000000000000000, -315.0000000000000000 ) ) ;
#5923 = CARTESIAN_POINT ( 'NONE',  ( 9.142617743994909674, -7.997268146336696581, -315.0000000000000568 ) ) ;
#5924 = VERTEX_POINT ( 'NONE', #9992 ) ;
#5925 = CARTESIAN_POINT ( 'NONE',  ( -98.44423576012317767, -2.500000000000000000, -338.7741350709160315 ) ) ;
#5926 = LINE ( 'NONE', #9421, #6946 ) ;
#5927 = VERTEX_POINT ( 'NONE', #5149 ) ;
#5928 = CARTESIAN_POINT ( 'NONE',  ( -18.87000901094000227, 1.611639242563999819, -317.5000000000470095 ) ) ;
#5929 = ORIENTED_EDGE ( 'NONE', *, *, #6050, .T. ) ;
#5930 = CARTESIAN_POINT ( 'NONE',  ( 16.06911929583999310, 5.954958506906000260, -317.4928077629770087 ) ) ;
#5931 =( GEOMETRIC_REPRESENTATION_CONTEXT ( 3 ) GLOBAL_UNCERTAINTY_ASSIGNED_CONTEXT ( ( #4102 ) ) GLOBAL_UNIT_ASSIGNED_CONTEXT ( ( #6052, #9240, #5294 ) ) REPRESENTATION_CONTEXT ( 'NONE', 'WORKASPACE' ) );
#5932 = EDGE_CURVE ( 'NONE', #6229, #3553, #9647, .T. ) ;
#5933 = CARTESIAN_POINT ( 'NONE',  ( -17.60469080286000931, -4.126100741655001514, -317.4928077629770087 ) ) ;
#5934 = CARTESIAN_POINT ( 'NONE',  ( -17.59298685096999648, 0.02218567204014999794, -314.4150829855000211 ) ) ;
#5935 = B_SPLINE_CURVE_WITH_KNOTS ( 'NONE', 3,
 ( #5878, #3369, #2559, #7502, #3419, #6697, #9975 ),
 .UNSPECIFIED., .F., .F.,
 ( 4, 1, 1, 1, 4 ),
 ( 0.000000000000000000, 0.2500000000000000000, 0.5000000000000000000, 0.7500000000000000000, 1.000000000000000000 ),
 .UNSPECIFIED. ) ;
#5936 = SURFACE_SIDE_STYLE ('',( #7056 ) ) ;
#5937 = COLOUR_RGB ( '', 0.72549020, 0.75294118, 0.79215686) ;
#5938 = EDGE_CURVE ( 'NONE', #1584, #2824, #8603, .T. ) ;
#5939 = CARTESIAN_POINT ( 'NONE',  ( 15.91674550148000122, 7.581266318323002906, -303.6197174156520759 ) ) ;
#5940 = CARTESIAN_POINT ( 'NONE',  ( -17.44863594367627613, -0.8973220716409442410, 314.4999502393482089 ) ) ;
#5941 = EDGE_LOOP ( 'NONE', ( #3021, #6810, #6910, #3297 ) ) ;
#5942 = CARTESIAN_POINT ( 'NONE',  ( -17.11849373668000140, -0.6181952683021000317, -314.8616023057000461 ) ) ;
#5943 = EDGE_CURVE ( 'NONE', #8573, #215, #6773, .T. ) ;
#5944 = CARTESIAN_POINT ( 'NONE',  ( -6.594989095229207621, -7.500000000000000000, -526.5005977704149700 ) ) ;
#5945 = EDGE_LOOP ( 'NONE', ( #7614, #8450, #6249, #10027 ) ) ;
#5946 = CARTESIAN_POINT ( 'NONE',  ( 19.85617711436999144, -1.942822351932998792, 190.4207385301700128 ) ) ;
#5947 = CARTESIAN_POINT ( 'NONE',  ( -46.74071243419621169, -9.500000000000001776, -414.3237589990241077 ) ) ;
#5948 = LINE ( 'NONE', #5136, #1888 ) ;
#5949 = CARTESIAN_POINT ( 'NONE',  ( -19.77421425755001039, 1.922351829117000976, 191.1197171614399792 ) ) ;
#5950 = CARTESIAN_POINT ( 'NONE',  ( 15.27200851150000105, -4.387263554753999983, 314.8616023057000461 ) ) ;
#5951 = EDGE_CURVE ( 'NONE', #3089, #5548, #9081, .T. ) ;
#5952 = CARTESIAN_POINT ( 'NONE',  ( -10.00000000000000000, -2.500000000000000000, -272.5000000000000000 ) ) ;
#5953 = CARTESIAN_POINT ( 'NONE',  ( 18.32873049326003212, -4.258249849688001909, 320.0770942683900557 ) ) ;
#5954 = CARTESIAN_POINT ( 'NONE',  ( 9.378959784071181360, -5.899999999999999467, -525.1866552614185366 ) ) ;
#5955 = CARTESIAN_POINT ( 'NONE',  ( 17.71378747801019315, 5.838323448755804002, -303.5000000000000000 ) ) ;
#5956 = CARTESIAN_POINT ( 'NONE',  ( 16.78232460783999969, 3.056336161456999712, 314.4150829855000211 ) ) ;
#5957 = VERTEX_POINT ( 'NONE', #9300 ) ;
#5958 = CYLINDRICAL_SURFACE ( 'NONE', #4492, 3.500000000000003109 ) ;
#5959 = CARTESIAN_POINT ( 'NONE',  ( 7.868470208275999411, 11.58296045169998401, 319.5792614743400009 ) ) ;
#5960 = DIRECTION ( 'NONE',  ( 3.596898303937126455E-07, 0.9999999999999354960, -1.203273141451894460E-22 ) ) ;
#5961 = AXIS2_PLACEMENT_3D ( 'NONE', #3403, #4415, #2703 ) ;
#5962 = CARTESIAN_POINT ( 'NONE',  ( 11.28384026436728327, 7.096146896414363248, 315.0000000000000000 ) ) ;
#5963 = DIRECTION ( 'NONE',  ( 0.9942380540931650135, 0.000000000000000000, 0.1071946444232960011 ) ) ;
#5964 = ORIENTED_EDGE ( 'NONE', *, *, #9309, .T. ) ;
#5965 = CARTESIAN_POINT ( 'NONE',  ( -1.379544352527027007, -2.545980799917907600, -434.5827932828950679 ) ) ;
#5966 = CARTESIAN_POINT ( 'NONE',  ( 15.00000000000326139, -5.136019918588313243E-17, 315.0000000000001137 ) ) ;
#5967 = FACE_OUTER_BOUND ( 'NONE', #3519, .T. ) ;
#5968 = CARTESIAN_POINT ( 'NONE',  ( 16.24773438692637839, -3.756014664266052350, 314.4999406160053468 ) ) ;
#5969 = CARTESIAN_POINT ( 'NONE',  ( 18.45932313982999062, 2.405278989253002209, 190.0071920248299477 ) ) ;
#5970 = AXIS2_PLACEMENT_3D ( 'NONE', #2103, #7956, #9463 ) ;
#5971 = DIRECTION ( 'NONE',  ( -0.9712267471052614676, 0.000000000000000000, -0.2381566831044902022 ) ) ;
#5972 = CARTESIAN_POINT ( 'NONE',  ( 8.500452883955736283, -4.229385977086412396, -525.6786231025552070 ) ) ;
#5973 = DIRECTION ( 'NONE',  ( 0.7784864941890659029, 0.000000000000000000, 0.6276613564377032661 ) ) ;
#5974 = LINE ( 'NONE', #8285, #1183 ) ;
#5975 = EDGE_LOOP ( 'NONE', ( #300, #10291, #5226, #6483 ) ) ;
#5976 = CARTESIAN_POINT ( 'NONE',  ( 16.80239380511999059, 5.162410948549997158, 319.9928079742500131 ) ) ;
#5977 = DIRECTION ( 'NONE',  ( 0.4712473909295827323, 0.000000000000000000, -0.8820010751365675583 ) ) ;
#5978 = ORIENTED_EDGE ( 'NONE', *, *, #5221, .T. ) ;
#5979 = DIRECTION ( 'NONE',  ( 0.000000000000000000, -1.000000000000000000, 0.000000000000000000 ) ) ;
#5980 = ORIENTED_EDGE ( 'NONE', *, *, #1426, .F. ) ;
#5981 = CARTESIAN_POINT ( 'NONE',  ( -15.24853452200002302, 6.688806263293003873, -317.4928077629770087 ) ) ;
#5982 = CARTESIAN_POINT ( 'NONE',  ( 15.24853452200002302, -6.688806263293003873, -317.4928077629770087 ) ) ;
#5983 = CARTESIAN_POINT ( 'NONE',  ( -17.56954514911999965, -0.4333932196220000033, -314.4150829855000211 ) ) ;
#5984 = CARTESIAN_POINT ( 'NONE',  ( -119.6503683519543983, -7.500000000000000000, -299.0840866897705155 ) ) ;
#5985 = LINE ( 'NONE', #8762, #2580 ) ;
#5986 = ORIENTED_EDGE ( 'NONE', *, *, #3790, .T. ) ;
#5987 = CARTESIAN_POINT ( 'NONE',  ( 3.134365345935000047, -11.35765845234000082, 190.0000000000000000 ) ) ;
#5988 = AXIS2_PLACEMENT_3D ( 'NONE', #3911, #6492, #7404 ) ;
#5989 = AXIS2_PLACEMENT_3D ( 'NONE', #5082, #3265, #5832 ) ;
#5990 = DIRECTION ( 'NONE',  ( 5.235554895604999868E-10, 4.130578887848000029E-10, 1.000000000000000000 ) ) ;
#5991 =( REPRESENTATION_RELATIONSHIP ('NONE','NONE', #8468, #4020 ) REPRESENTATION_RELATIONSHIP_WITH_TRANSFORMATION ( #6559 )SHAPE_REPRESENTATION_RELATIONSHIP( ) );
#5992 = ORIENTED_EDGE ( 'NONE', *, *, #5820, .T. ) ;
#5993 = LINE ( 'NONE', #5189, #1926 ) ;
#5994 = FACE_OUTER_BOUND ( 'NONE', #5550, .T. ) ;
#5995 = CARTESIAN_POINT ( 'NONE',  ( 4.866278641173998665, -11.00354869785000211, -302.5071922382879279 ) ) ;
#5996 = CARTESIAN_POINT ( 'NONE',  ( -16.34052447997000357, 7.211013068275999416, 191.1197171614399792 ) ) ;
#5997 = PRODUCT_RELATED_PRODUCT_CATEGORY ( 'part', '', ( #381 ) ) ;
#5998 = CARTESIAN_POINT ( 'NONE',  ( -1.924873525447142519, -7.449631413182002504, -434.7394372756328949 ) ) ;
#5999 = DIRECTION ( 'NONE',  ( -0.8820010751365675583, 0.000000000000000000, -0.4712473909295827323 ) ) ;
#6000 = CARTESIAN_POINT ( 'NONE',  ( 4.404324556173000005, -12.28809208595000335, 319.5792614743400009 ) ) ;
#6001 = DIRECTION ( 'NONE',  ( 0.000000000000000000, -1.000000000000000000, 0.000000000000000000 ) ) ;
#6002 = CARTESIAN_POINT ( 'NONE',  ( 17.14577796628000073, -0.02050488658304999712, -314.8616023057000461 ) ) ;
#6003 = CARTESIAN_POINT ( 'NONE',  ( 15.07109120124999890, 4.275483045295999318, 315.0848619657999734 ) ) ;
#6004 = EDGE_LOOP ( 'NONE', ( #9156, #3997, #6373, #2289, #3314 ) ) ;
#6005 = DIRECTION ( 'NONE',  ( 0.000000000000000000, -1.000000000000000000, 0.000000000000000000 ) ) ;
#6006 = CARTESIAN_POINT ( 'NONE',  ( 17.10170768143997932, 6.605950023609995725, 319.5792614743400009 ) ) ;
#6007 = EDGE_CURVE ( 'NONE', #2874, #320, #5689, .T. ) ;
#6008 = EDGE_CURVE ( 'NONE', #10392, #1085, #4692, .T. ) ;
#6009 = CARTESIAN_POINT ( 'NONE',  ( -7.536255787234116710, -3.385256688352999088, -438.0084054756555929 ) ) ;
#6010 = CIRCLE ( 'NONE', #3442, 3.500000000000003109 ) ;
#6011 = CARTESIAN_POINT ( 'NONE',  ( -8.096811247556559010, 8.344189070382460827, 315.0000000000001137 ) ) ;
#6012 = CARTESIAN_POINT ( 'NONE',  ( -86.49427212956700828, -7.500000000000000000, -350.5299153184531633 ) ) ;
#6013 = CIRCLE ( 'NONE', #6533, 10.00000000000000000 ) ;
#6014 = CARTESIAN_POINT ( 'NONE',  ( -1.267742039733871229, -2.539130078730544415, -434.5353378591038904 ) ) ;
#6015 = FACE_BOUND ( 'NONE', #5975, .T. ) ;
#6016 = CARTESIAN_POINT ( 'NONE',  ( 18.99997815069999874, 0.3119984768183999835, 190.0000000000100044 ) ) ;
#6017 = EDGE_CURVE ( 'NONE', #1207, #2603, #4606, .T. ) ;
#6018 = CARTESIAN_POINT ( 'NONE',  ( 6.176507221981585971, -9.366274586590517259, 314.4999436549671259 ) ) ;
#6019 = CARTESIAN_POINT ( 'NONE',  ( 16.23266328071998643, 5.782092517776998619, 190.0071920248299477 ) ) ;
#6020 = DIRECTION ( 'NONE',  ( -0.7494507079133034821, 0.000000000000000000, 0.6620601456123518247 ) ) ;
#6021 = EDGE_CURVE ( 'NONE', #911, #2578, #4666, .T. ) ;
#6022 = CARTESIAN_POINT ( 'NONE',  ( 6.675319431708749640, -4.451976413186169879, -525.2453362690079075 ) ) ;
#6023 =( GEOMETRIC_REPRESENTATION_CONTEXT ( 3 ) GLOBAL_UNCERTAINTY_ASSIGNED_CONTEXT ( ( #6354 ) ) GLOBAL_UNIT_ASSIGNED_CONTEXT ( ( #713, #1625, #4206 ) ) REPRESENTATION_CONTEXT ( 'NONE', 'WORKASPACE' ) );
#6024 = LINE ( 'NONE', #10163, #2194 ) ;
#6025 = UNCERTAINTY_MEASURE_WITH_UNIT (LENGTH_MEASURE( 1.000000000000000082E-05 ), #8367, 'distance_accuracy_value', 'NONE');
#6026 = DIRECTION ( 'NONE',  ( 0.000000000000000000, 0.000000000000000000, -1.000000000000000000 ) ) ;
#6027 = ORIENTED_EDGE ( 'NONE', *, *, #8297, .T. ) ;
#6028 = CARTESIAN_POINT ( 'NONE',  ( 18.86318716375000193, -0.4770217013004998119, 319.9928079742500131 ) ) ;
#6029 = CARTESIAN_POINT ( 'NONE',  ( -13.36185104356876785, -8.000000000000000000, -400.1641368440833730 ) ) ;
#6030 = DIRECTION ( 'NONE',  ( 0.000000000000000000, -1.000000000000000000, 0.000000000000000000 ) ) ;
#6031 = ORIENTED_EDGE ( 'NONE', *, *, #2809, .F. ) ;
#6032 = CARTESIAN_POINT ( 'NONE',  ( -1.983867121666000877, 11.33269556189999960, -317.4928077629770087 ) ) ;
#6033 = CARTESIAN_POINT ( 'NONE',  ( 2.028805552265000589, -12.03060078454999449, -317.5770954168139610 ) ) ;
#6034 = EDGE_CURVE ( 'NONE', #5350, #9268, #5457, .T. ) ;
#6035 = PRODUCT ( 'Pivot Pin', 'Pivot Pin', '', ( #8063 ) ) ;
#6036 = AXIS2_PLACEMENT_3D ( 'NONE', #2798, #9362, #5312 ) ;
#6037 = CARTESIAN_POINT ( 'NONE',  ( -15.43693218238999876, 4.538485726840999490, -314.6383426456000052 ) ) ;
#6038 = CARTESIAN_POINT ( 'NONE',  ( 11.52006393673606865, 7.476351274249532608, -314.5677505184611391 ) ) ;
#6039 = CARTESIAN_POINT ( 'NONE',  ( 17.49922277440664686, -0.09424638433143421590, 314.4999507458385892 ) ) ;
#6040 = VERTEX_POINT ( 'NONE', #9349 ) ;
#6041 = CARTESIAN_POINT ( 'NONE',  ( 17.80781204382000027, -3.997739559166000323, 190.0000000000000000 ) ) ;
#6042 = CARTESIAN_POINT ( 'NONE',  ( -46.74071243416547361, -2.500000000000000000, -414.3237589990478114 ) ) ;
#6043 = ORIENTED_EDGE ( 'NONE', *, *, #9291, .T. ) ;
#6044 = CARTESIAN_POINT ( 'NONE',  ( -20.00478054794001537, -0.07382975964156003601, 191.1197171614399792 ) ) ;
#6045 = EDGE_LOOP ( 'NONE', ( #3358, #3085 ) ) ;
#6046 = DIRECTION ( 'NONE',  ( 0.000000000000000000, 1.000000000000000000, 0.000000000000000000 ) ) ;
#6047 = CARTESIAN_POINT ( 'NONE',  ( -119.6503683519543983, -2.500000000000000000, -299.0840866897705155 ) ) ;
#6048 = CARTESIAN_POINT ( 'NONE',  ( 19.97288175887001316, -0.5556452136295997324, 191.1197171614399792 ) ) ;
#6049 = AXIS2_PLACEMENT_3D ( 'NONE', #5306, #1225, #9452 ) ;
#6050 = EDGE_CURVE ( 'NONE', #982, #5064, #7753, .T. ) ;
#6051 = LINE ( 'NONE', #2884, #4087 ) ;
#6052 =( LENGTH_UNIT ( ) NAMED_UNIT ( * ) SI_UNIT ( .MILLI., .METRE. ) );
#6053 = DIRECTION ( 'NONE',  ( -0.2833167629018695233, 0.000000000000000000, 0.9590263874674178624 ) ) ;
#6054 = CIRCLE ( 'NONE', #2801, 0.5000000000000172085 ) ;
#6055 = CARTESIAN_POINT ( 'NONE',  ( -17.71262672283002360, -5.941112223585997221, 319.5792614743400009 ) ) ;
#6056 = FACE_OUTER_BOUND ( 'NONE', #1471, .T. ) ;
#6057 = CARTESIAN_POINT ( 'NONE',  ( -15.74033075358999945, 3.452242816619000010, 315.0848619657999734 ) ) ;
#6058 = EDGE_LOOP ( 'NONE', ( #4770, #2866, #905, #764 ) ) ;
#6059 = DIRECTION ( 'NONE',  ( -0.7426245373609573486, 0.000000000000000000, 0.6697079934638857646 ) ) ;
#6060 = ORIENTED_EDGE ( 'NONE', *, *, #4489, .T. ) ;
#6061 = CARTESIAN_POINT ( 'NONE',  ( -10.97158218462999457, 10.45285060525999121, 318.8802828394900644 ) ) ;
#6062 = B_SPLINE_SURFACE_WITH_KNOTS ( 'NONE', 3, 3, ( 
 ( #5071, #7497, #9165, #5983 ),
 ( #139, #1043, #9327, #4329 ),
 ( #10024, #9380, #7656, #5934 ),
 ( #8352, #9277, #8508, #296 ),
 ( #3414, #9224, #7704, #7602 ),
 ( #4278, #5873, #2014, #5182 ),
 ( #2611, #249, #3526, #6803 ),
 ( #990, #348, #10076, #8455 ),
 ( #1095, #10124, #6037, #1961 ),
 ( #1296, #3662, #10165, #6952 ),
 ( #1347, #6131, #6898, #4576 ),
 ( #5319, #5269, #2808, #7004 ),
 ( #10226, #7850, #10276, #2861 ),
 ( #497, #7901, #3765, #2161 ),
 ( #8761, #7058, #546, #7960 ),
 ( #10322, #1242, #2913, #3616 ),
 ( #1401, #6081, #3822, #2964 ),
 ( #4685, #2212, #6181, #6235 ),
 ( #2106, #2005, #9371, #8544 ),
 ( #4518, #7797, #1187, #8653 ),
 ( #10376, #9465, #7745, #9522 ),
 ( #4630, #3016, #4466, #9418 ),
 ( #7107, #388, #2054, #8593 ),
 ( #443, #5427, #8703, #6290 ),
 ( #9574, #5481, #3718, #5372 ),
 ( #4844, #6400, #10589, #8014 ),
 ( #6561, #9843, #2265, #7264 ),
 ( #756, #3981, #6, #5749 ),
 ( #2321, #5532, #7157, #10536 ),
 ( #2480, #710, #8815, #8983 ),
 ( #3179, #6453, #1623, #10478 ),
 ( #9034, #8118, #4894, #4945 ),
 ( #4041, #8872, #9733, #607 ),
 ( #1672, #3068, #808, #7319 ) ),
 .UNSPECIFIED., .F., .F., .F.,
 ( 4, 1, 1, 1, 1, 1, 1, 1, 1, 1, 1, 1, 1, 1, 1, 1, 1, 1, 1, 1, 1, 1, 1, 1, 1, 1, 1, 1, 1, 1, 1, 4 ),
 ( 4, 4 ),
 ( -0.01402646298304000005, 0.000000000000000000, 0.03448275862069000164, 0.06896551724138000328, 0.1034482758621000087, 0.1379310344828000023, 0.1724137931033999926, 0.2068965517240999863, 0.2413793103448000077, 0.2758620689655000291, 0.3103448275861999672, 0.3448275862069000164, 0.3793103448276000100, 0.4137931034483000037, 0.4482758620689999973, 0.4827586206897000465, 0.5172413793103000090, 0.5517241379310000582, 0.5862068965516999963, 0.6206896551723999345, 0.6551724137930999836, 0.6896551724138000328, 0.7241379310344999709, 0.7586206896552000201, 0.7931034482758999582, 0.8275862068966000074, 0.8620689655171999144, 0.8965517241379000746, 0.9310344827586000127, 0.9655172413793000619, 1.000000000000000000, 1.015741306098000063 ),
 ( -0.1697239316932999953, 1.169834029081999960 ),
 .UNSPECIFIED. ) ;
#6063 = EDGE_CURVE ( 'NONE', #4799, #4588, #1985, .T. ) ;
#6064 = FACE_OUTER_BOUND ( 'NONE', #191, .T. ) ;
#6065 = CARTESIAN_POINT ( 'NONE',  ( -16.25530297147532721, 2.761162301196854685, 315.0000000000000000 ) ) ;
#6066 = CARTESIAN_POINT ( 'NONE',  ( 15.00000000000072120, -0.4945770392355430256, 315.0000000000001705 ) ) ;
#6067 = CARTESIAN_POINT ( 'NONE',  ( 17.50000000000000000, 0.000000000000000000, -315.0000000000000000 ) ) ;
#6068 = ADVANCED_FACE ( 'NONE', ( #9548 ), #6628, .T. ) ;
#6069 = LINE ( 'NONE', #10216, #6775 ) ;
#6070 = AXIS2_PLACEMENT_3D ( 'NONE', #3749, #9720, #10310 ) ;
#6071 = CARTESIAN_POINT ( 'NONE',  ( -38.59226537204000351, -2.500000000000000000, -500.7880554352000217 ) ) ;
#6072 = EDGE_CURVE ( 'NONE', #2769, #5378, #9483, .T. ) ;
#6073 = CARTESIAN_POINT ( 'NONE',  ( -16.91992689674541950, 1.077645906677548115, -315.0000000000000000 ) ) ;
#6074 = CARTESIAN_POINT ( 'NONE',  ( 0.6878067384150999830, 11.39249343872000075, 190.0071920248299477 ) ) ;
#6075 = CARTESIAN_POINT ( 'NONE',  ( -80.80421425739181984, -2.500000000000000000, -329.3491872523243842 ) ) ;
#6076 = AXIS2_PLACEMENT_3D ( 'NONE', #5376, #8818, #3826 ) ;
#6077 = CARTESIAN_POINT ( 'NONE',  ( 13.36995595564000006, -8.154012700520999246, -317.5000000000000000 ) ) ;
#6078 = VECTOR ( 'NONE', #6119, 1000.000000000000000 ) ;
#6079 = DIRECTION ( 'NONE',  ( 0.9942380540931650135, 0.000000000000000000, 0.1071946444232960011 ) ) ;
#6080 = CARTESIAN_POINT ( 'NONE',  ( 5.334308159457383347, -9.025045582129868293, 314.9999999999999432 ) ) ;
#6081 = CARTESIAN_POINT ( 'NONE',  ( -1.399029207469000058, 9.644928263550999858, -314.8616023057000461 ) ) ;
#6082 = EDGE_CURVE ( 'NONE', #4372, #4635, #3683, .T. ) ;
#6083 = ORIENTED_EDGE ( 'NONE', *, *, #7787, .F. ) ;
#6084 = CARTESIAN_POINT ( 'NONE',  ( 18.87181153733000016, -0.3572136203155001355, 319.9928079742500131 ) ) ;
#6085 = CARTESIAN_POINT ( 'NONE',  ( 17.74479464825532204, -5.801447790587960895, -316.5000000000004547 ) ) ;
#6086 = CARTESIAN_POINT ( 'NONE',  ( -15.54870946350325767, -7.500000000000000000, -436.1258788022018393 ) ) ;
#6087 = ORIENTED_EDGE ( 'NONE', *, *, #2998, .T. ) ;
#6088 = VECTOR ( 'NONE', #889, 1000.000000000000000 ) ;
#6089 = STYLED_ITEM ( 'NONE', ( #6605 ), #5170 ) ;
#6090 = DIRECTION ( 'NONE',  ( 0.9942380540931649024, 0.000000000000000000, 0.1071946444232959872 ) ) ;
#6091 = AXIS2_PLACEMENT_3D ( 'NONE', #8674, #4485, #1368 ) ;
#6092 = CARTESIAN_POINT ( 'NONE',  ( 10.62478234909000285, -10.68521885564000051, -317.0792622552969533 ) ) ;
#6093 = CARTESIAN_POINT ( 'NONE',  ( -20.57979856674000629, -2.500000000000000000, -389.8948508258000061 ) ) ;
#6094 = CARTESIAN_POINT ( 'NONE',  ( 28.53863984632670636, -7.500000000000000000, -506.8274460463252353 ) ) ;
#6095 = ORIENTED_EDGE ( 'NONE', *, *, #670, .F. ) ;
#6096 = COLOUR_RGB ( '', 0.66274510, 0.83137255, 0.94901961) ;
#6097 = LINE ( 'NONE', #2069, #2667 ) ;
#6098 = ORIENTED_EDGE ( 'NONE', *, *, #2048, .F. ) ;
#6099 = CARTESIAN_POINT ( 'NONE',  ( -9.971838575284008854, -10.83713921150001447, 191.1197171614399792 ) ) ;
#6100 = ORIENTED_EDGE ( 'NONE', *, *, #6953, .T. ) ;
#6101 = CARTESIAN_POINT ( 'NONE',  ( -16.37177374402162400, -2.538919766875962658, 314.9999999999999432 ) ) ;
#6102 = CARTESIAN_POINT ( 'NONE',  ( -12.29914730983998972, -8.615864166288998760, -302.5071922382879279 ) ) ;
#6103 = CARTESIAN_POINT ( 'NONE',  ( 19.98293839508998104, -0.4162045188173000287, 191.1197171614399792 ) ) ;
#6104 = AXIS2_PLACEMENT_3D ( 'NONE', #6129, #9971, #2159 ) ;
#6105 = CARTESIAN_POINT ( 'NONE',  ( -1.015842471293257887, -7.493001980645002114, -434.3570987632741094 ) ) ;
#6106 = CARTESIAN_POINT ( 'NONE',  ( 13.31171245337000819, 8.049428572247000702, -302.5071922382879279 ) ) ;
#6107 = CARTESIAN_POINT ( 'NONE',  ( 20.04253597850999569, -0.9484392003694999129, 319.5792614743400009 ) ) ;
#6108 = CARTESIAN_POINT ( 'NONE',  ( 17.21448334449999962, -1.351716521078000222, -314.6383426456000052 ) ) ;
#6109 = CARTESIAN_POINT ( 'NONE',  ( -16.76545246634000108, 2.037063237379999947, 314.8616023057000461 ) ) ;
#6110 = ORIENTED_EDGE ( 'NONE', *, *, #3985, .F. ) ;
#6111 = CARTESIAN_POINT ( 'NONE',  ( 16.21588929933999523, -5.798404451932999137, 190.0071920248299477 ) ) ;
#6112 = CARTESIAN_POINT ( 'NONE',  ( -7.493827757249003518, 11.59400354817999457, 318.8802828394900644 ) ) ;
#6113 = CARTESIAN_POINT ( 'NONE',  ( -15.00000000000000000, 0.000000000000000000, -285.0000000000000000 ) ) ;
#6114 = ORIENTED_EDGE ( 'NONE', *, *, #6388, .T. ) ;
#6115 = LINE ( 'NONE', #5408, #9917 ) ;
#6116 = FACE_OUTER_BOUND ( 'NONE', #6745, .T. ) ;
#6117 = CARTESIAN_POINT ( 'NONE',  ( -2.814980436929585108E-10, -12.50000000000000000, 319.0000000000000000 ) ) ;
#6118 = CARTESIAN_POINT ( 'NONE',  ( 19.51225877040622692, 2.792229942217316463, 319.0000000000005116 ) ) ;
#6119 = DIRECTION ( 'NONE',  ( 0.000000000000000000, 1.000000000000000000, 0.000000000000000000 ) ) ;
#6120 = ADVANCED_FACE ( 'NONE', ( #9335 ), #5390, .T. ) ;
#6121 = CARTESIAN_POINT ( 'NONE',  ( -13.10769442058508716, -5.671717519033600219, -438.3867234666666945 ) ) ;
#6122 = CARTESIAN_POINT ( 'NONE',  ( -5.242074483217283642, 9.033702059254421712, -315.0000000000000000 ) ) ;
#6123 = CARTESIAN_POINT ( 'NONE',  ( 4.308829118669001979, 11.09213725138999962, 190.0071920248299477 ) ) ;
#6124 = CARTESIAN_POINT ( 'NONE',  ( -86.49427212956700828, -2.500000000000000000, -350.5299153184531633 ) ) ;
#6125 = ADVANCED_FACE ( 'NONE', ( #1917 ), #3633, .T. ) ;
#6126 = LINE ( 'NONE', #10162, #4263 ) ;
#6127 = EDGE_CURVE ( 'NONE', #8053, #4605, #5993, .T. ) ;
#6128 = CARTESIAN_POINT ( 'NONE',  ( -1.582650547086741799, -7.339339277715000165, -435.1382983596024019 ) ) ;
#6129 = CARTESIAN_POINT ( 'NONE',  ( 0.000000000000000000, 0.000000000000000000, 0.000000000000000000 ) ) ;
#6130 = CARTESIAN_POINT ( 'NONE',  ( 1.962900534989000745, -9.435972684515721909, 314.9999999999999432 ) ) ;
#6131 = CARTESIAN_POINT ( 'NONE',  ( -13.37260572687999982, 6.041714840053000302, -314.8616023057000461 ) ) ;
#6132 = EDGE_LOOP ( 'NONE', ( #5079, #5714, #1247, #1509 ) ) ;
#6133 = AXIS2_PLACEMENT_3D ( 'NONE', #5166, #1136, #3454 ) ;
#6134 = CARTESIAN_POINT ( 'NONE',  ( 18.89057790499001754, 0.06397434778252002185, 319.9928079742500131 ) ) ;
#6135 = CARTESIAN_POINT ( 'NONE',  ( -17.71658133615935427, -5.834976589818515080, -316.5000000000004547 ) ) ;
#6136 = CYLINDRICAL_SURFACE ( 'NONE', #1411, 12.49999999999998579 ) ;
#6137 = ORIENTED_EDGE ( 'NONE', *, *, #7510, .F. ) ;
#6138 = CARTESIAN_POINT ( 'NONE',  ( 17.49999999954662044, -9.625715914672042649E-06, 190.0000000000000000 ) ) ;
#6139 = CARTESIAN_POINT ( 'NONE',  ( 8.115185848843001537, -11.51636271397001465, -317.0792622552969533 ) ) ;
#6140 = CYLINDRICAL_SURFACE ( 'NONE', #9632, 3.499999999999997335 ) ;
#6141 = EDGE_CURVE ( 'NONE', #9430, #2509, #1482, .T. ) ;
#6142 = CARTESIAN_POINT ( 'NONE',  ( -5.416173751597343156, -8.000000000000000000, -337.7825848737071510 ) ) ;
#6143 = ORIENTED_EDGE ( 'NONE', *, *, #4174, .F. ) ;
#6144 = CARTESIAN_POINT ( 'NONE',  ( 17.34597251029000375, -4.674348096672999553, 190.0000000000000000 ) ) ;
#6145 = CARTESIAN_POINT ( 'NONE',  ( -10.23467949917770525, -9.999999999493892844, 189.9999999999997726 ) ) ;
#6146 = VERTEX_POINT ( 'NONE', #4002 ) ;
#6147 = CARTESIAN_POINT ( 'NONE',  ( 1.248913580286000302, -12.48838264809999643, 191.1197171614399792 ) ) ;
#6148 = EDGE_LOOP ( 'NONE', ( #8606, #2112, #1599, #1353, #2274, #8092, #8018 ) ) ;
#6149 = FACE_OUTER_BOUND ( 'NONE', #8956, .T. ) ;
#6150 = CARTESIAN_POINT ( 'NONE',  ( 3.306880204566999382, -11.21686954173999951, -302.5071922382879279 ) ) ;
#6151 = EDGE_CURVE ( 'NONE', #4003, #8834, #2267, .T. ) ;
#6152 = CARTESIAN_POINT ( 'NONE',  ( -14.96977070983867009, -9.633703999999999823, -385.2505660326773409 ) ) ;
#6153 = DIRECTION ( 'NONE',  ( 0.6276613564376841703, 0.000000000000000000, -0.7784864941890811130 ) ) ;
#6154 = CARTESIAN_POINT ( 'NONE',  ( -85.79375217459825365, -2.500000000000000000, -343.3529193039154279 ) ) ;
#6155 = CARTESIAN_POINT ( 'NONE',  ( 14.79708307774000353, -8.514882941861998233, 319.5792614743400009 ) ) ;
#6156 = CARTESIAN_POINT ( 'NONE',  ( 16.28527389671999970, -3.844447514156999812, -314.4150829855000211 ) ) ;
#6157 = CARTESIAN_POINT ( 'NONE',  ( -17.12243801299000268, 0.5826713957640000663, 314.8616023057000461 ) ) ;
#6158 = ORIENTED_EDGE ( 'NONE', *, *, #2869, .T. ) ;
#6159 = CARTESIAN_POINT ( 'NONE',  ( 15.60334176867001688, -6.376785739494004623, 190.0071920248299477 ) ) ;
#6160 = CARTESIAN_POINT ( 'NONE',  ( -0.8314117387865108677, -7.488021948898482272, -434.3195962711836842 ) ) ;
#6161 = CARTESIAN_POINT ( 'NONE',  ( -14.37110465573396212, -7.500000000000000000, -348.9812360766022721 ) ) ;
#6162 = AXIS2_PLACEMENT_3D ( 'NONE', #8938, #6410, #5602 ) ;
#6163 = EDGE_CURVE ( 'NONE', #7707, #269, #1755, .T. ) ;
#6164 = CARTESIAN_POINT ( 'NONE',  ( -43.24071243418999444, 2.500000000000000000, -414.3237589990000629 ) ) ;
#6165 = DIRECTION ( 'NONE',  ( 0.000000000000000000, -1.000000000000000000, 0.000000000000000000 ) ) ;
#6166 = CARTESIAN_POINT ( 'NONE',  ( 0.000000000000000000, -7.937240849781000307, 315.0000000000001705 ) ) ;
#6167 = CIRCLE ( 'NONE', #692, 0.5000000000000004441 ) ;
#6168 = CARTESIAN_POINT ( 'NONE',  ( 6.052780067456072999, -5.500000000000000000, -524.2189112390747141 ) ) ;
#6169 = CARTESIAN_POINT ( 'NONE',  ( -20.00000000000000000, -7.771159141713679452E-11, 319.0000000000000000 ) ) ;
#6170 = DIRECTION ( 'NONE',  ( 0.000000000000000000, 1.000000000000000000, 0.000000000000000000 ) ) ;
#6171 = PLANE ( 'NONE',  #719 ) ;
#6172 = CARTESIAN_POINT ( 'NONE',  ( -8.666289393444031930, 8.161235200486094854, -315.0000000000000000 ) ) ;
#6173 = DIRECTION ( 'NONE',  ( 0.9627070496199739980, 0.1321637200910051047, 0.2360675490272045873 ) ) ;
#6174 = CARTESIAN_POINT ( 'NONE',  ( -84.02975002432511076, -7.500000000000000000, -342.4104245220563030 ) ) ;
#6175 = VECTOR ( 'NONE', #7353, 1000.000000000000000 ) ;
#6176 = ADVANCED_FACE ( 'NONE', ( #1419 ), #8140, .F. ) ;
#6177 = EDGE_LOOP ( 'NONE', ( #6724, #3957, #2772, #6954 ) ) ;
#6178 = CARTESIAN_POINT ( 'NONE',  ( 11.32071836301000012, -9.223563301002998926, -317.5000000000000000 ) ) ;
#6179 = CARTESIAN_POINT ( 'NONE',  ( -2.000000000003786749, -9.500000000000001776, -409.4999999999758415 ) ) ;
#6180 = CARTESIAN_POINT ( 'NONE',  ( 16.34899991413091414, -2.583752171356570759, 315.0000000000000000 ) ) ;
#6181 = CARTESIAN_POINT ( 'NONE',  ( 1.276003512426000075, 9.874146089817999794, -314.6383426456000052 ) ) ;
#6182 = CARTESIAN_POINT ( 'NONE',  ( -17.50000000000125056, -1.380497925828168986E-12, -314.4963898845654171 ) ) ;
#6183 = LINE ( 'NONE', #7799, #6887 ) ;
#6184 = DIRECTION ( 'NONE',  ( -0.2951854283188049544, 0.000000000000000000, 0.9554399839384176696 ) ) ;
#6185 = ORIENTED_EDGE ( 'NONE', *, *, #7641, .F. ) ;
#6186 = CARTESIAN_POINT ( 'NONE',  ( -16.58827648083000028, 6.426222433883002516, -317.5770954168139610 ) ) ;
#6187 =( BOUNDED_SURFACE ( )  B_SPLINE_SURFACE ( 3, 3, ( 
 ( #1693, #8243, #2503, #3301, #7496, #5769, #5179, #7548, #5982, #9276, #5016, #3363, #3467, #193, #28, #6639, #9057, #4968, #84, #5819, #7599, #4220, #935, #2553, #8294, #9112, #4381, #137, #1092, #3413, #6749, #9968, #10023, #4166, #2665, #5933, #2716, #2609, #5872, #9223, #1855 ),
 ( #10075, #9163, #1908, #247, #5125, #1746, #8402, #1042, #1802, #5070, #8453, #3525, #8351, #6583, #989, #4276, #4328, #6802, #9866, #6033, #7703, #5435, #7805, #2062, #9325, #9426, #4525, #1147, #9528, #8712, #2114, #347, #6188, #7065, #3773, #1959, #5230, #10123, #294, #4473, #2764 ),
 ( #2971, #6242, #2012, #3625, #450, #3725, #7654, #6905, #8506, #4426, #10173, #2816, #4583, #6092, #7859, #6139, #9378, #5326, #5278, #8552, #1249, #9473, #7011, #1355, #2168, #3572, #1196, #10330, #504, #10282, #7752, #2920, #395, #3668, #6961, #10235, #6853, #5380, #2868, #8601, #8661 ),
 ( #1304, #8824, #1409, #6297, #4750, #717, #1469, #4854, #5539, #8129, #2273, #8020, #614, #2221, #6515, #8879, #10543, #10597, #663, #3939, #3990, #4693, #7164, #3888, #10435, #553, #6460, #7115, #9798, #3187, #10383, #9582, #4638, #7220, #7968, #5490, #10487, #7272, #3129, #766, #6407 ) ),
 .UNSPECIFIED., .F., .F., .F. ) 
 B_SPLINE_SURFACE_WITH_KNOTS ( ( 4, 4 ),
 ( 4, 1, 1, 1, 1, 1, 1, 1, 1, 1, 1, 1, 1, 1, 1, 1, 1, 1, 1, 1, 1, 1, 1, 1, 1, 1, 1, 1, 1, 1, 1, 1, 1, 1, 1, 1, 1, 1, 4 ),
 ( 0.000000000000000000, 1.000000000000000000 ),
 ( -0.007738640450445999699, 0.000000000000000000, 0.03414709649185000001, 0.06696605908318999101, 0.09596079224771000837, 0.1211002772268999911, 0.1443783404606999998, 0.1680876537897000034, 0.1921286104184000143, 0.2160216200219000071, 0.2397245863996999848, 0.2634813019505999887, 0.2879188160025000220, 0.3133917475886000004, 0.3395543376315999784, 0.3663618195672999622, 0.3946229251345000355, 0.4252536485549999745, 0.4591139563344999730, 0.4956048897295999844, 0.5324779435423999674, 0.5674158629142000976, 0.5992726300609999557, 0.6287198090143000240, 0.6565915576515000129, 0.6836661054489000522, 0.7100337132233999204, 0.7353920520230999847, 0.7598724402797999433, 0.7838392479475999597, 0.8076909583479000565, 0.8317349054331000247, 0.8555088018188000687, 0.8788217029082999732, 0.9039691640437000908, 0.9329692239710999369, 0.9658153655582000230, 1.000000000000000000, 1.008464120473999914 ),
 .UNSPECIFIED. ) 
 GEOMETRIC_REPRESENTATION_ITEM ( )  RATIONAL_B_SPLINE_SURFACE ( (
 ( 1.236577356246000070, 1.236577356246000070, 1.236577356246000070, 1.236577356246000070, 1.236577356246000070, 1.236577356246000070, 1.236577356246000070, 1.236577356246000070, 1.236577356246000070, 1.236577356246000070, 1.236577356246000070, 1.236577356246000070, 1.236577356246000070, 1.236577356246000070, 1.236577356246000070, 1.236577356246000070, 1.236577356246000070, 1.236577356246000070, 1.236577356246000070, 1.236577356246000070, 1.236577356246000070, 1.236577356246000070, 1.236577356246000070, 1.236577356246000070, 1.236577356246000070, 1.236577356246000070, 1.236577356246000070, 1.236577356246000070, 1.236577356246000070, 1.236577356246000070, 1.236577356246000070, 1.236577356246000070, 1.236577356246000070, 1.236577356246000070, 1.236577356246000070, 1.236577356246000070, 1.236577356246000070, 1.236577356246000070, 1.236577356246000070, 1.236577356246000070, 1.236577356246000070),
 ( 0.9211408812511999722, 0.9211408812511999722, 0.9211408812511999722, 0.9211408812511999722, 0.9211408812511999722, 0.9211408812511999722, 0.9211408812511999722, 0.9211408812511999722, 0.9211408812511999722, 0.9211408812511999722, 0.9211408812511999722, 0.9211408812511999722, 0.9211408812511999722, 0.9211408812511999722, 0.9211408812511999722, 0.9211408812511999722, 0.9211408812511999722, 0.9211408812511999722, 0.9211408812511999722, 0.9211408812511999722, 0.9211408812511999722, 0.9211408812511999722, 0.9211408812511999722, 0.9211408812511999722, 0.9211408812511999722, 0.9211408812511999722, 0.9211408812511999722, 0.9211408812511999722, 0.9211408812511999722, 0.9211408812511999722, 0.9211408812511999722, 0.9211408812511999722, 0.9211408812511999722, 0.9211408812511999722, 0.9211408812511999722, 0.9211408812511999722, 0.9211408812511999722, 0.9211408812511999722, 0.9211408812511999722, 0.9211408812511999722, 0.9211408812511999722),
 ( 0.9211408812511999722, 0.9211408812511999722, 0.9211408812511999722, 0.9211408812511999722, 0.9211408812511999722, 0.9211408812511999722, 0.9211408812511999722, 0.9211408812511999722, 0.9211408812511999722, 0.9211408812511999722, 0.9211408812511999722, 0.9211408812511999722, 0.9211408812511999722, 0.9211408812511999722, 0.9211408812511999722, 0.9211408812511999722, 0.9211408812511999722, 0.9211408812511999722, 0.9211408812511999722, 0.9211408812511999722, 0.9211408812511999722, 0.9211408812511999722, 0.9211408812511999722, 0.9211408812511999722, 0.9211408812511999722, 0.9211408812511999722, 0.9211408812511999722, 0.9211408812511999722, 0.9211408812511999722, 0.9211408812511999722, 0.9211408812511999722, 0.9211408812511999722, 0.9211408812511999722, 0.9211408812511999722, 0.9211408812511999722, 0.9211408812511999722, 0.9211408812511999722, 0.9211408812511999722, 0.9211408812511999722, 0.9211408812511999722, 0.9211408812511999722),
 ( 1.236577356246000070, 1.236577356246000070, 1.236577356246000070, 1.236577356246000070, 1.236577356246000070, 1.236577356246000070, 1.236577356246000070, 1.236577356246000070, 1.236577356246000070, 1.236577356246000070, 1.236577356246000070, 1.236577356246000070, 1.236577356246000070, 1.236577356246000070, 1.236577356246000070, 1.236577356246000070, 1.236577356246000070, 1.236577356246000070, 1.236577356246000070, 1.236577356246000070, 1.236577356246000070, 1.236577356246000070, 1.236577356246000070, 1.236577356246000070, 1.236577356246000070, 1.236577356246000070, 1.236577356246000070, 1.236577356246000070, 1.236577356246000070, 1.236577356246000070, 1.236577356246000070, 1.236577356246000070, 1.236577356246000070, 1.236577356246000070, 1.236577356246000070, 1.236577356246000070, 1.236577356246000070, 1.236577356246000070, 1.236577356246000070, 1.236577356246000070, 1.236577356246000070) ) ) 
 REPRESENTATION_ITEM ( '' )  SURFACE ( )  );
#6188 = CARTESIAN_POINT ( 'NONE',  ( -15.65816392223999820, -7.257913545763996055, -317.5770954168139610 ) ) ;
#6189 = B_SPLINE_CURVE_WITH_KNOTS ( 'NONE', 3,
 ( #9640, #3837, #10388, #9750, #6302, #9586, #3892, #5495, #8774, #10441, #1417, #5656, #10556, #4699, #3082, #6358, #2282, #5546, #8835, #4215, #7333, #7438, #3357, #8345, #5713, #9107, #76, #1638, #1794, #7491, #9859, #4270, #7540, #2548, #6577, #6683, #10016, #2443, #6634, #8237, #5065, #8190, #4160, #9910, #983, #5119 ),
 .UNSPECIFIED., .F., .F.,
 ( 4, 2, 2, 2, 2, 2, 2, 2, 2, 2, 2, 2, 2, 2, 2, 2, 2, 2, 2, 2, 2, 2, 4 ),
 ( 0.000000000000000000, 0.001362852592701297230, 0.002044278889051945412, 0.002725705185402593159, 0.004088557778103890823, 0.005451410370805188921, 0.006814262963506486151, 0.008177115556207781646, 0.01090282074161037437, 0.01635423111241555635, 0.01907993629781814388, 0.02180564148322073487, 0.02453134666862332586, 0.02725705185402591685, 0.02998275703942850437, 0.03270846222483109189, 0.03543416741023368288, 0.03815987259563628081, 0.03952272518833757631, 0.04088557778103886486, 0.04224843037374016036, 0.04292985667009080464, 0.04361128296644144198 ),
 .UNSPECIFIED. ) ;
#6190 = CARTESIAN_POINT ( 'NONE',  ( -31.97945899169042505, -7.500000000000000000, -498.3127369250419747 ) ) ;
#6191 = DIRECTION ( 'NONE',  ( -0.000000000000000000, 1.000000000000000000, 0.000000000000000000 ) ) ;
#6192 = ORIENTED_EDGE ( 'NONE', *, *, #7629, .F. ) ;
#6193 = CARTESIAN_POINT ( 'NONE',  ( -14.96977070983867009, -9.500000000000001776, -385.2505660326773409 ) ) ;
#6194 = ADVANCED_FACE ( 'NONE', ( #3142 ), #8837, .T. ) ;
#6195 = CARTESIAN_POINT ( 'NONE',  ( -19.79155829785255349, -1.881978406165077500, 319.0000000000003979 ) ) ;
#6196 = ORIENTED_EDGE ( 'NONE', *, *, #363, .T. ) ;
#6197 = CARTESIAN_POINT ( 'NONE',  ( -19.97288175887001316, 0.5556452136296999855, 191.1197171614399792 ) ) ;
#6198 = ORIENTED_EDGE ( 'NONE', *, *, #757, .T. ) ;
#6199 = CARTESIAN_POINT ( 'NONE',  ( -15.75886148104574325, -3.542954957252464343, 315.0000000000000000 ) ) ;
#6200 = FACE_OUTER_BOUND ( 'NONE', #6607, .T. ) ;
#6201 = CARTESIAN_POINT ( 'NONE',  ( 18.20422786544000715, 5.185156308378004120, 191.1197171614399792 ) ) ;
#6202 = VECTOR ( 'NONE', #7201, 1000.000000000000000 ) ;
#6203 = LINE ( 'NONE', #3638, #1331 ) ;
#6204 = SURFACE_STYLE_FILL_AREA ( #2077 ) ;
#6205 = EDGE_CURVE ( 'NONE', #56, #3871, #10341, .T. ) ;
#6206 = CARTESIAN_POINT ( 'NONE',  ( -4.866278641173998665, 11.00354869785000211, -302.5071922382879279 ) ) ;
#6207 = CARTESIAN_POINT ( 'NONE',  ( -18.77791317464001608, -4.479224074632002228, 319.5792614743400009 ) ) ;
#6208 = AXIS2_PLACEMENT_3D ( 'NONE', #1038, #4162, #1690 ) ;
#6209 = ADVANCED_FACE ( 'NONE', ( #3949 ), #7917, .T. ) ;
#6210 = CARTESIAN_POINT ( 'NONE',  ( -6.488017178959999853, 9.182784307579000327, 314.6383426456000052 ) ) ;
#6211 = AXIS2_PLACEMENT_3D ( 'NONE', #9895, #4142, #59 ) ;
#6212 = ORIENTED_EDGE ( 'NONE', *, *, #9764, .F. ) ;
#6213 = CARTESIAN_POINT ( 'NONE',  ( -11.56561186376999295, -8.976555918559004255, 190.0071920248299477 ) ) ;
#6214 = ORIENTED_EDGE ( 'NONE', *, *, #7921, .F. ) ;
#6215 = CARTESIAN_POINT ( 'NONE',  ( -18.17597206675998223, 5.223702392620001689, 318.8802828394900644 ) ) ;
#6216 = PLANE ( 'NONE',  #845 ) ;
#6217 = VECTOR ( 'NONE', #9723, 1000.000000000000114 ) ;
#6218 = CARTESIAN_POINT ( 'NONE',  ( -17.34710322845000263, 0.4172063223308000168, 314.6383426456000052 ) ) ;
#6219 = CARTESIAN_POINT ( 'NONE',  ( -9.285088343770869557, -9.000000000000001776, -419.6576319987959778 ) ) ;
#6220 = CARTESIAN_POINT ( 'NONE',  ( -15.40286302630929427, 3.995001727760178145, 315.0000000000000568 ) ) ;
#6221 = CARTESIAN_POINT ( 'NONE',  ( -7.006889269069000115, -6.844138725329000472, 315.0000000000001705 ) ) ;
#6222 = CARTESIAN_POINT ( 'NONE',  ( -15.42284054825286610, -3.971008657351323468, -314.9999999999998863 ) ) ;
#6223 = CARTESIAN_POINT ( 'NONE',  ( -2.807317995047950987, -2.838317565875291937, -435.7570541054141131 ) ) ;
#6224 = CARTESIAN_POINT ( 'NONE',  ( -12.86189865087530038, -4.241237746457299451, -438.9337381460082952 ) ) ;
#6225 = CARTESIAN_POINT ( 'NONE',  ( 1.499999999999999556, 2.500000000000000000, -409.5000000000000568 ) ) ;
#6226 = CARTESIAN_POINT ( 'NONE',  ( -5.850354798305519743, 8.918567588720486938, -315.0000000000000568 ) ) ;
#6227 = CARTESIAN_POINT ( 'NONE',  ( 19.38229133873998222, 1.780473529460998128, 189.9229057364800042 ) ) ;
#6228 = CARTESIAN_POINT ( 'NONE',  ( -17.50000000000001776, 8.653894624238266756E-10, 189.9999999999998863 ) ) ;
#6229 = VERTEX_POINT ( 'NONE', #5608 ) ;
#6230 = CARTESIAN_POINT ( 'NONE',  ( 16.90341843474000072, -5.241942252742000541, -317.4999999999989768 ) ) ;
#6231 = DIRECTION ( 'NONE',  ( 0.1283609399493171599, 0.9912279006826364425, 0.03147567320362416182 ) ) ;
#6232 = AXIS2_PLACEMENT_3D ( 'NONE', #2302, #4610, #3916 ) ;
#6233 = CARTESIAN_POINT ( 'NONE',  ( 0.000000000000000000, 0.000000000000000000, 0.000000000000000000 ) ) ;
#6234 = CARTESIAN_POINT ( 'NONE',  ( 11.65165375873240450, -6.897932327036405020, 315.0000000000000568 ) ) ;
#6235 = CARTESIAN_POINT ( 'NONE',  ( 1.285290206351000108, 10.09749793447999977, -314.4150829855000211 ) ) ;
#6236 = CARTESIAN_POINT ( 'NONE',  ( 17.49922277440664686, -0.09424638433143421590, 315.0000000000000000 ) ) ;
#6237 = CARTESIAN_POINT ( 'NONE',  ( 12.95511329522999233, 9.055231460430995583, 320.0770942683900557 ) ) ;
#6238 = DIRECTION ( 'NONE',  ( 0.8820010751365678914, 0.000000000000000000, 0.4712473909295818442 ) ) ;
#6239 = CARTESIAN_POINT ( 'NONE',  ( -0.7241641665009055373, -2.498143066284999936, -434.1460077833778541 ) ) ;
#6240 = EDGE_LOOP ( 'NONE', ( #8071, #6580 ) ) ;
#6241 = CARTESIAN_POINT ( 'NONE',  ( -2.028805552265000589, 12.03060078454999449, -317.5770954168139610 ) ) ;
#6242 = CARTESIAN_POINT ( 'NONE',  ( 20.06704520635998179, 0.4211730678688000440, -317.0792622552969533 ) ) ;
#6243 = PRESENTATION_LAYER_ASSIGNMENT (  '', '', ( #8299 ) ) ;
#6244 = CIRCLE ( 'NONE', #3672, 10.00000000000000533 ) ;
#6245 = CARTESIAN_POINT ( 'NONE',  ( -46.74071243416547361, -7.500000000000000000, -414.3237589990478114 ) ) ;
#6246 = CARTESIAN_POINT ( 'NONE',  ( 6.877779018054728688, -2.500000000000000000, -527.5833393823892266 ) ) ;
#6247 = AXIS2_PLACEMENT_3D ( 'NONE', #2055, #8595, #2709 ) ;
#6249 = ORIENTED_EDGE ( 'NONE', *, *, #2872, .T. ) ;
#6248 = AXIS2_PLACEMENT_3D ( 'NONE', #3231, #9678, #658 ) ;
#6250 = CARTESIAN_POINT ( 'NONE',  ( 9.378959784071181360, -4.100000000000000533, -525.1866552614185366 ) ) ;
#6251 = PLANE ( 'NONE',  #9357 ) ;
#6252 = CIRCLE ( 'NONE', #9009, 15.00000000000002309 ) ;
#6253 = EDGE_CURVE ( 'NONE', #6326, #5811, #1529, .T. ) ;
#6254 = ORIENTED_EDGE ( 'NONE', *, *, #2542, .F. ) ;
#6255 = CARTESIAN_POINT ( 'NONE',  ( -11.75848697160781064, 10.12394145745024510, -316.5000000000004547 ) ) ;
#6256 = ORIENTED_EDGE ( 'NONE', *, *, #1160, .T. ) ;
#6257 = CARTESIAN_POINT ( 'NONE',  ( 19.99999721801999897, 7.771189452710000131E-11, 191.0000000000000000 ) ) ;
#6258 = CARTESIAN_POINT ( 'NONE',  ( -17.39204038057999924, -5.566020924881995846, -302.4229045757450081 ) ) ;
#6259 = CARTESIAN_POINT ( 'NONE',  ( 19.96348645057001647, 0.8966426439394996617, 191.1197171614399792 ) ) ;
#6260 = EDGE_CURVE ( 'NONE', #7297, #3286, #8120, .T. ) ;
#6261 = CARTESIAN_POINT ( 'NONE',  ( -1.433262749849905537, -7.342401167152001307, -434.9822336619507723 ) ) ;
#6262 = SHAPE_REPRESENTATION_RELATIONSHIP ( 'NONE' , 'NONE' ,  #6273, #3778 ) ;
#6263 = EDGE_CURVE ( 'NONE', #4067, #10485, #8399, .T. ) ;
#6264 = CARTESIAN_POINT ( 'NONE',  ( -81.08127826530241578, -2.500000000000000000, -352.1729300552810855 ) ) ;
#6265 = CARTESIAN_POINT ( 'NONE',  ( -65.06086774174146115, -7.500000000000000888, -381.4479802647836664 ) ) ;
#6266 = CARTESIAN_POINT ( 'NONE',  ( -12.10743226551000085, -7.094093637544000686, -314.6383426456000052 ) ) ;
#6267 = CARTESIAN_POINT ( 'NONE',  ( -8.690073206612000334, 8.569658446474999636, 314.6383426456000052 ) ) ;
#6268 = ORIENTED_EDGE ( 'NONE', *, *, #9945, .F. ) ;
#6269 = CARTESIAN_POINT ( 'NONE',  ( -72.90663470102438737, -7.500000000000000888, -371.7168990826883714 ) ) ;
#6270 = CARTESIAN_POINT ( 'NONE',  ( -1.627435584940745361, -7.438904789989194022, -434.6825096147837826 ) ) ;
#6271 = CYLINDRICAL_SURFACE ( 'NONE', #5665, 0.7499999999999997780 ) ;
#6272 = MECHANICAL_DESIGN_GEOMETRIC_PRESENTATION_REPRESENTATION (  '', ( #3188 ), #9707 ) ;
#6273 = SHAPE_REPRESENTATION ( 'Lower Jaw Base Arm', ( #2817 ), #7476 ) ;
#6274 = EDGE_CURVE ( 'NONE', #5389, #5957, #7424, .T. ) ;
#6275 = PLANE ( 'NONE',  #1684 ) ;
#6276 = CARTESIAN_POINT ( 'NONE',  ( -16.95014751240671913, 0.8318069206872661381, 315.0000000000000000 ) ) ;
#6277 = CARTESIAN_POINT ( 'NONE',  ( -18.45919443845001950, -2.405475664342000996, 319.9928079742500131 ) ) ;
#6278 = PRODUCT_DEFINITION_FORMATION_WITH_SPECIFIED_SOURCE ( 'ANY', '', #1924, .NOT_KNOWN. ) ;
#6279 = CARTESIAN_POINT ( 'NONE',  ( 19.99999721132999753, -3.518697978483000342E-10, 319.0000000000000000 ) ) ;
#6280 = CARTESIAN_POINT ( 'NONE',  ( -6.872637154772029078, -3.412160298610301012, -437.2496588370372592 ) ) ;
#6281 = SURFACE_SIDE_STYLE ('',( #3811 ) ) ;
#6282 = CARTESIAN_POINT ( 'NONE',  ( -5.517019332057546244, -6.998165768227002204, -437.5004988621744246 ) ) ;
#6283 = CARTESIAN_POINT ( 'NONE',  ( -1.574054099965566111, 9.469115279523554918, -315.0000000000001705 ) ) ;
#6284 = CARTESIAN_POINT ( 'NONE',  ( -3.087789584922997932, 11.94493704178999671, 189.9229057364800042 ) ) ;
#6285 = CARTESIAN_POINT ( 'NONE',  ( -1.582652182125599660, -2.660653890702000091, -435.1382991101020821 ) ) ;
#6286 = DIRECTION ( 'NONE',  ( 0.000000000000000000, 1.000000000000000000, -0.000000000000000000 ) ) ;
#6287 = VECTOR ( 'NONE', #5916, 1000.000000000000000 ) ;
#6288 = CARTESIAN_POINT ( 'NONE',  ( 6.052780067456072999, -4.500000000000000888, -524.2189112390747141 ) ) ;
#6289 = CARTESIAN_POINT ( 'NONE',  ( 16.47320456655591059, -2.338720490045835820, 314.9999999999999432 ) ) ;
#6290 = CARTESIAN_POINT ( 'NONE',  ( 13.56771446467999986, 6.451120369226999607, -314.4150829855000211 ) ) ;
#6291 = CARTESIAN_POINT ( 'NONE',  ( 17.40348243411531826, -5.898854857574459487, 315.0000000000000000 ) ) ;
#6292 = CARTESIAN_POINT ( 'NONE',  ( -19.54690800120000205, 0.8885403386512999990, 320.0770942683900557 ) ) ;
#6293 = CARTESIAN_POINT ( 'NONE',  ( -2.000000000000000000, 4.200000000000000178, -409.5000000000000000 ) ) ;
#6294 = CARTESIAN_POINT ( 'NONE',  ( -0.2842986807686446182, -2.455579271718999035, -434.1368229023160552 ) ) ;
#6295 = ORIENTED_EDGE ( 'NONE', *, *, #5002, .F. ) ;
#6296 = CARTESIAN_POINT ( 'NONE',  ( -13.97631948628000309, 9.047145764649998867, -317.0792622552969533 ) ) ;
#6297 = CARTESIAN_POINT ( 'NONE',  ( 19.87640215697998158, -1.702148751976998442, -316.3802825947000201 ) ) ;
#6298 = FACE_BOUND ( 'NONE', #502, .T. ) ;
#6299 = AXIS2_PLACEMENT_3D ( 'NONE', #10010, #282, #8439 ) ;
#6300 = DIRECTION ( 'NONE',  ( 0.8820010751365675583, 0.000000000000000000, 0.4712473909295827323 ) ) ;
#6301 = ORIENTED_EDGE ( 'NONE', *, *, #10494, .T. ) ;
#6302 = CARTESIAN_POINT ( 'NONE',  ( -17.20152651095805041, -1.793788947124295374, -314.5180462286797365 ) ) ;
#6303 = ORIENTED_EDGE ( 'NONE', *, *, #786, .T. ) ;
#6304 = CARTESIAN_POINT ( 'NONE',  ( 7.865580335751168661, 11.50505378538359125, -316.5000000000004547 ) ) ;
#6305 = VERTEX_POINT ( 'NONE', #9001 ) ;
#6306 = CARTESIAN_POINT ( 'NONE',  ( -15.52919946924948569, -3.840693445095582081, 314.9999999999999432 ) ) ;
#6307 = CARTESIAN_POINT ( 'NONE',  ( -12.85183647427999176, -9.678193536939003749, -302.9207377450070453 ) ) ;
#6308 = DIRECTION ( 'NONE',  ( 0.000000000000000000, 1.000000000000000000, 0.000000000000000000 ) ) ;
#6309 = CARTESIAN_POINT ( 'NONE',  ( 17.39204038057999924, 5.566020924881995846, -302.4229045757450081 ) ) ;
#6310 = DIRECTION ( 'NONE',  ( 0.9921831154218024862, -0.000000000000000000, 0.1247904863035890766 ) ) ;
#6311 = VERTEX_POINT ( 'NONE', #6636 ) ;
#6312 = CARTESIAN_POINT ( 'NONE',  ( -15.56325459994999960, -4.731967449628999844, -314.4150829855000211 ) ) ;
#6313 = CARTESIAN_POINT ( 'NONE',  ( 12.33444409538000031, 8.732262621622000509, -302.5000000000000000 ) ) ;
#6314 = EDGE_LOOP ( 'NONE', ( #8882, #3787, #2171, #6083 ) ) ;
#6315 = CARTESIAN_POINT ( 'NONE',  ( -16.06942734036999454, -6.898991720969999797, 189.9229057364800042 ) ) ;
#6316 = CARTESIAN_POINT ( 'NONE',  ( 14.79888371878075048, 8.420183212156704400, 190.9999999999996589 ) ) ;
#6317 = PRODUCT_RELATED_PRODUCT_CATEGORY ( 'part', '', ( #10331 ) ) ;
#6318 = PLANE ( 'NONE',  #5154 ) ;
#6319 = CARTESIAN_POINT ( 'NONE',  ( -13.18712987686000027, -5.898505050745000311, 315.0848619657999734 ) ) ;
#6320 = CARTESIAN_POINT ( 'NONE',  ( 17.49922277440664686, -0.09424638433143421590, 315.0000000000000000 ) ) ;
#6321 = CARTESIAN_POINT ( 'NONE',  ( 12.63876572971000023, 8.567575428377999458, 320.0000000000000000 ) ) ;
#6322 = CARTESIAN_POINT ( 'NONE',  ( -6.240232637630001911, -10.74449313720999832, 319.9928079742500131 ) ) ;
#6323 = CARTESIAN_POINT ( 'NONE',  ( -13.82248977823974734, -5.505663031471445201, -315.0000000000000000 ) ) ;
#6324 = SURFACE_STYLE_USAGE ( .BOTH. , #3056 ) ;
#6325 = CARTESIAN_POINT ( 'NONE',  ( -37.87192209818999800, 2.500000000000000000, -461.0868123482000556 ) ) ;
#6326 = VERTEX_POINT ( 'NONE', #9912 ) ;
#6327 = DIRECTION ( 'NONE',  ( 0.9936574763089276452, 0.000000000000000000, 0.1124491875265132140 ) ) ;
#6328 = AXIS2_PLACEMENT_3D ( 'NONE', #6652, #6597, #5083 ) ;
#6329 = AXIS2_PLACEMENT_3D ( 'NONE', #1486, #4867, #4763 ) ;
#6330 = EDGE_CURVE ( 'NONE', #6416, #5654, #555, .T. ) ;
#6331 = APPLICATION_CONTEXT ( 'automotive_design' ) ;
#6332 = CARTESIAN_POINT ( 'NONE',  ( -19.19804233804001115, 3.716674010855997690, 190.4207385301700128 ) ) ;
#6333 = CARTESIAN_POINT ( 'NONE',  ( 5.118368704603114087E-10, 10.00000000003099210, 314.4999681336588537 ) ) ;
#6334 = LINE ( 'NONE', #5691, #1510 ) ;
#6335 = CIRCLE ( 'NONE', #1194, 3.500000000000003109 ) ;
#6336 = VECTOR ( 'NONE', #678, 1000.000000000000000 ) ;
#6337 = DIRECTION ( 'NONE',  ( -0.4712473909295827323, 0.000000000000000000, 0.8820010751365675583 ) ) ;
#6338 = APPLICATION_PROTOCOL_DEFINITION ( 'draft international standard', 'automotive_design', 1998, #4147 ) ;
#6339 = CARTESIAN_POINT ( 'NONE',  ( -8.032401884333960851, -11.45915766226284482, -303.4999999999996589 ) ) ;
#6340 = CARTESIAN_POINT ( 'NONE',  ( -72.90663470102438737, -12.40000000000001101, -368.2168990826883146 ) ) ;
#6341 = ADVANCED_FACE ( 'NONE', ( #2445 ), #2550, .T. ) ;
#6342 = CARTESIAN_POINT ( 'NONE',  ( 10.19111349739211292, -9.999999999041103038, 314.4999507458385324 ) ) ;
#6343 = EDGE_CURVE ( 'NONE', #5064, #982, #2098, .T. ) ;
#6344 = CARTESIAN_POINT ( 'NONE',  ( -15.30440697208000600, 7.531500302410004011, 320.0770942683900557 ) ) ;
#6345 = CARTESIAN_POINT ( 'NONE',  ( -14.84121504900874911, -5.582427545768324784, -439.0111117078143934 ) ) ;
#6346 = CARTESIAN_POINT ( 'NONE',  ( -1.029674599165786741, -2.507553075840000645, -434.3642002394484507 ) ) ;
#6347 = ORIENTED_EDGE ( 'NONE', *, *, #5848, .T. ) ;
#6348 = CARTESIAN_POINT ( 'NONE',  ( 17.39473599676002635, 5.562790558317003864, -317.5770954168139610 ) ) ;
#6349 = VECTOR ( 'NONE', #1463, 1000.000000000000000 ) ;
#6350 = PLANE ( 'NONE',  #10289 ) ;
#6351 = ORIENTED_EDGE ( 'NONE', *, *, #9742, .T. ) ;
#6352 = CARTESIAN_POINT ( 'NONE',  ( -15.54870946350325767, -7.500000000000000000, -436.1258788022018393 ) ) ;
#6353 = ORIENTED_EDGE ( 'NONE', *, *, #9179, .T. ) ;
#6354 = UNCERTAINTY_MEASURE_WITH_UNIT (LENGTH_MEASURE( 1.000000000000000082E-05 ), #713, 'distance_accuracy_value', 'NONE');
#6355 = AXIS2_PLACEMENT_3D ( 'NONE', #7190, #3100, #742 ) ;
#6356 = PLANE ( 'NONE',  #2966 ) ;
#6357 = EDGE_LOOP ( 'NONE', ( #7542, #4495, #7074, #8734 ) ) ;
#6358 = CARTESIAN_POINT ( 'NONE',  ( -12.32755932899231688, -7.043638358067994432, -314.5741798689286384 ) ) ;
#6359 = ADVANCED_FACE ( 'NONE', ( #2606 ), #134, .F. ) ;
#6360 = EDGE_LOOP ( 'NONE', ( #7465, #6095, #5672, #1170 ) ) ;
#6361 = CARTESIAN_POINT ( 'NONE',  ( 17.71658133615935782, 5.834976589818514192, -316.5000000000004547 ) ) ;
#6362 = ORIENTED_EDGE ( 'NONE', *, *, #3844, .F. ) ;
#6363 = CARTESIAN_POINT ( 'NONE',  ( -15.24035984457677628, -4.192874667847209302, 315.0000000000000000 ) ) ;
#6364 = CARTESIAN_POINT ( 'NONE',  ( -6.704579698891996564, -11.86746000475999452, -302.9207377450070453 ) ) ;
#6365 = DIRECTION ( 'NONE',  ( 0.000000000000000000, -1.000000000000000000, 0.000000000000000000 ) ) ;
#6366 = VERTEX_POINT ( 'NONE', #2660 ) ;
#6367 = VECTOR ( 'NONE', #556, 1000.000000000000000 ) ;
#6368 = CARTESIAN_POINT ( 'NONE',  ( -17.42451203059000520, 5.527343733032997974, -302.4229045757450081 ) ) ;
#6369 = CARTESIAN_POINT ( 'NONE',  ( 9.912528015309003848, -10.85837313990000474, 318.8802828394900644 ) ) ;
#6370 = ORIENTED_EDGE ( 'NONE', *, *, #9690, .F. ) ;
#6371 = CARTESIAN_POINT ( 'NONE',  ( 6.488017178959999853, -9.182784307579000327, -314.6383426456000052 ) ) ;
#6372 = CARTESIAN_POINT ( 'NONE',  ( -2.040568488410468895, -2.585414927994879264, -434.8398312044259342 ) ) ;
#6373 = ORIENTED_EDGE ( 'NONE', *, *, #4443, .T. ) ;
#6374 = CARTESIAN_POINT ( 'NONE',  ( 11.98038374875001111, -9.553300872651998787, 189.9229057364800042 ) ) ;
#6375 = CARTESIAN_POINT ( 'NONE',  ( -14.83495203015046116, 8.394818437327874250, 190.9999999999996589 ) ) ;
#6376 = LINE ( 'NONE', #2462, #6175 ) ;
#6377 = ORIENTED_EDGE ( 'NONE', *, *, #7985, .T. ) ;
#6378 = VECTOR ( 'NONE', #216, 1000.000000000000000 ) ;
#6379 = CARTESIAN_POINT ( 'NONE',  ( -8.519003879469000395, -8.390442916014999142, 314.8616023057000461 ) ) ;
#6380 =( NAMED_UNIT ( * ) PLANE_ANGLE_UNIT ( ) SI_UNIT ( $, .RADIAN. ) );
#6381 = CYLINDRICAL_SURFACE ( 'NONE', #1243, 3.500000000000020428 ) ;
#6382 = CARTESIAN_POINT ( 'NONE',  ( -72.90663470102438737, -2.500000000000000000, -375.1168990826883487 ) ) ;
#6383 = CARTESIAN_POINT ( 'NONE',  ( 13.15646768860627169, 9.424872508248352432, 319.0000000000005116 ) ) ;
#6384 = CARTESIAN_POINT ( 'NONE',  ( -14.74684780783305449, -4.500000000000000888, -439.3959507452315165 ) ) ;
#6385 = CARTESIAN_POINT ( 'NONE',  ( -101.9722400606694350, -2.500000000000000000, -340.6591246346343382 ) ) ;
#6386 = ORIENTED_EDGE ( 'NONE', *, *, #7743, .F. ) ;
#6387 = CARTESIAN_POINT ( 'NONE',  ( -14.00000000000000000, 2.500000000000000000, -317.5000000000000000 ) ) ;
#6388 = EDGE_CURVE ( 'NONE', #7389, #8266, #9824, .T. ) ;
#6389 = PRODUCT_DEFINITION_SHAPE ( 'NONE', 'NONE',  #10633 ) ;
#6390 = CARTESIAN_POINT ( 'NONE',  ( -18.75098855781002882, 3.495875360606998772, 189.9229057364800042 ) ) ;
#6391 = CARTESIAN_POINT ( 'NONE',  ( 10.23467949917770525, 9.999999999493887515, -302.4999999999997158 ) ) ;
#6392 = VECTOR ( 'NONE', #3639, 1000.000000000000227 ) ;
#6393 = ORIENTED_EDGE ( 'NONE', *, *, #5619, .F. ) ;
#6394 = FACE_OUTER_BOUND ( 'NONE', #4690, .T. ) ;
#6395 = EDGE_CURVE ( 'NONE', #5334, #6718, #10119, .T. ) ;
#6396 = CARTESIAN_POINT ( 'NONE',  ( 16.99996037728000076, -1.352915776343000118E-09, 314.9999801883000146 ) ) ;
#6397 = ITEM_DEFINED_TRANSFORMATION ( 'NONE', 'NONE', #112,  #2817 ) ;
#6398 = CARTESIAN_POINT ( 'NONE',  ( -6.687916194383508817, -11.79215677264876838, -303.4999999999996589 ) ) ;
#6399 = ADVANCED_FACE ( 'NONE', ( #8503 ), #6136, .T. ) ;
#6400 = CARTESIAN_POINT ( 'NONE',  ( 15.23514566747999943, 4.427644513407000382, -314.8616023057000461 ) ) ;
#6401 = DIRECTION ( 'NONE',  ( 0.000000000000000000, -1.000000000000000000, 0.000000000000000000 ) ) ;
#6402 = CARTESIAN_POINT ( 'NONE',  ( 13.82465948680000878, 8.551125454139995696, 320.0770942683900557 ) ) ;
#6403 =( NAMED_UNIT ( * ) SI_UNIT ( $, .STERADIAN. ) SOLID_ANGLE_UNIT ( ) );
#6404 = CARTESIAN_POINT ( 'NONE',  ( -1.629498688047873012, -2.665385218676999290, -435.2813193451249276 ) ) ;
#6405 = ORIENTED_EDGE ( 'NONE', *, *, #6008, .T. ) ;
#6406 = CARTESIAN_POINT ( 'NONE',  ( -19.46922894822000316, 1.611824300579999925, -317.5770954168139610 ) ) ;
#6407 = CARTESIAN_POINT ( 'NONE',  ( -19.97262988322000865, 0.5553097472237004117, -316.3802825947000201 ) ) ;
#6408 = VECTOR ( 'NONE', #41, 1000.000000000000000 ) ;
#6409 = CARTESIAN_POINT ( 'NONE',  ( -1.295798468764000066, -11.49282963429000048, 320.0000000000000000 ) ) ;
#6410 = DIRECTION ( 'NONE',  ( 0.000000000000000000, 1.000000000000000000, 0.000000000000000000 ) ) ;
#6411 = LINE ( 'NONE', #3193, #4858 ) ;
#6412 = ORIENTED_EDGE ( 'NONE', *, *, #8864, .F. ) ;
#6413 = DIRECTION ( 'NONE',  ( 1.000000000000000000, 0.000000000000000000, 0.000000000000000000 ) ) ;
#6414 = ORIENTED_EDGE ( 'NONE', *, *, #770, .F. ) ;
#6415 = DIRECTION ( 'NONE',  ( -0.9902680687415799099, 0.000000000000000000, -0.1391731009599970204 ) ) ;
#6416 = VERTEX_POINT ( 'NONE', #4376 ) ;
#6417 = CARTESIAN_POINT ( 'NONE',  ( -13.97618761079829142, -5.383201530108604693, 314.9999999999999432 ) ) ;
#6418 = CARTESIAN_POINT ( 'NONE',  ( -3.702588368219998927, -12.37624192652999966, -302.9207377450070453 ) ) ;
#6419 = CARTESIAN_POINT ( 'NONE',  ( -82.96626782902075092, -7.500000000000000000, -348.6449257547347997 ) ) ;
#6420 = AXIS2_PLACEMENT_3D ( 'NONE', #2447, #831, #4110 ) ;
#6421 = CARTESIAN_POINT ( 'NONE',  ( -26.31853765676889267, -8.000000000000000000, -432.7407288192795249 ) ) ;
#6422 = VECTOR ( 'NONE', #3223, 1000.000000000000000 ) ;
#6423 = SHAPE_REPRESENTATION_RELATIONSHIP ( 'NONE' , 'NONE' ,  #33, #7250 ) ;
#6424 = PRESENTATION_LAYER_ASSIGNMENT (  '', '', ( #421 ) ) ;
#6425 = CARTESIAN_POINT ( 'NONE',  ( -18.93783568409002172, 3.175510411809001177, -302.4229045757450081 ) ) ;
#6426 = CARTESIAN_POINT ( 'NONE',  ( 8.771473555299991176, -11.23637119458999223, 318.8802828394900644 ) ) ;
#6427 = ORIENTED_EDGE ( 'NONE', *, *, #1807, .T. ) ;
#6428 = CARTESIAN_POINT ( 'NONE',  ( -13.18712987686000027, -5.898505050745000311, -315.0848619657999734 ) ) ;
#6429 = CARTESIAN_POINT ( 'NONE',  ( -17.35381917807999841, -0.3185724951638000402, 314.6383426456000052 ) ) ;
#6430 = ORIENTED_EDGE ( 'NONE', *, *, #3036, .F. ) ;
#6431 = CARTESIAN_POINT ( 'NONE',  ( 18.75098855781002882, -3.495875360606998772, 189.9229057364800042 ) ) ;
#6432 = CARTESIAN_POINT ( 'NONE',  ( -7.783073706837757122, 11.52583533951409933, 190.9999999999996589 ) ) ;
#6433 = DIRECTION ( 'NONE',  ( 0.000000000000000000, 1.000000000000000000, -0.000000000000000000 ) ) ;
#6434 = CIRCLE ( 'NONE', #10211, 5.000000000000004441 ) ;
#6435 = MECHANICAL_DESIGN_GEOMETRIC_PRESENTATION_REPRESENTATION (  '', ( #6089 ), #9695 ) ;
#6436 = CARTESIAN_POINT ( 'NONE',  ( -6.370857846455999507, -9.209451711050000711, 314.6383426456000052 ) ) ;
#6437 = CARTESIAN_POINT ( 'NONE',  ( 16.99996037728000076, -1.352915776343000118E-09, 314.9999801883000146 ) ) ;
#6438 = CARTESIAN_POINT ( 'NONE',  ( -18.20355969383999906, 3.293069710501999925, 320.0000000000000000 ) ) ;
#6439 = CARTESIAN_POINT ( 'NONE',  ( -2.000000000000000000, 2.500000000000000000, -406.0000000000000000 ) ) ;
#6440 = CARTESIAN_POINT ( 'NONE',  ( 14.04520818109275737, 8.909665382566956282, 319.0000000000005116 ) ) ;
#6441 = DIRECTION ( 'NONE',  ( 0.000000000000000000, -1.000000000000000000, 0.000000000000000000 ) ) ;
#6442 = CARTESIAN_POINT ( 'NONE',  ( -15.00000000000000000, 0.4945770392355999800, 315.0000000000000000 ) ) ;
#6443 = VERTEX_POINT ( 'NONE', #244 ) ;
#6444 = CARTESIAN_POINT ( 'NONE',  ( -86.49427212956700828, -2.500000000000000000, -350.5299153184531633 ) ) ;
#6445 =( GEOMETRIC_REPRESENTATION_CONTEXT ( 3 ) GLOBAL_UNCERTAINTY_ASSIGNED_CONTEXT ( ( #1950 ) ) GLOBAL_UNIT_ASSIGNED_CONTEXT ( ( #10396, #9593, #8618 ) ) REPRESENTATION_CONTEXT ( 'NONE', 'WORKASPACE' ) );
#6446 = CARTESIAN_POINT ( 'NONE',  ( -17.06589079541999965, 6.642208448352997507, 190.4207385301700128 ) ) ;
#6447 = DIRECTION ( 'NONE',  ( 0.000000000000000000, -1.000000000000000000, 0.000000000000000000 ) ) ;
#6448 = DIRECTION ( 'NONE',  ( 0.000000000000000000, 1.000000000000000000, 0.000000000000000000 ) ) ;
#6449 = PRODUCT_DEFINITION_FORMATION_WITH_SPECIFIED_SOURCE ( 'ANY', '', #8784, .NOT_KNOWN. ) ;
#6450 = CARTESIAN_POINT ( 'NONE',  ( 15.46063250253144972, 3.925225575964395919, 315.0000000000000568 ) ) ;
#6451 = PRODUCT_CONTEXT ( 'NONE', #9844, 'mechanical' ) ;
#6452 = CARTESIAN_POINT ( 'NONE',  ( 17.74743742734688112, -5.798256014711219208, -303.4999999999996589 ) ) ;
#6453 = CARTESIAN_POINT ( 'NONE',  ( 17.11849373668000140, 0.6181952683021999517, -314.8616023057000461 ) ) ;
#6454 = DIRECTION ( 'NONE',  ( 0.000000000000000000, 0.000000000000000000, 1.000000000000000000 ) ) ;
#6455 = CARTESIAN_POINT ( 'NONE',  ( -18.20429351259000228, 3.291556992836000006, 190.0000000000000000 ) ) ;
#6456 = CARTESIAN_POINT ( 'NONE',  ( 7.740399053647997185, 11.10168159160000201, 320.0770942683900557 ) ) ;
#6457 = CARTESIAN_POINT ( 'NONE',  ( -0.7400187527104828966, -2.555745218413001840, -434.6777242318867707 ) ) ;
#6458 = ORIENTED_EDGE ( 'NONE', *, *, #6021, .T. ) ;
#6459 = CARTESIAN_POINT ( 'NONE',  ( 16.84537440012000786, 6.754000406595005224, -316.3802825947000201 ) ) ;
#6460 = CARTESIAN_POINT ( 'NONE',  ( -9.192918156740001123, -11.10629030388999894, -316.3802825947000201 ) ) ;
#6461 = ORIENTED_EDGE ( 'NONE', *, *, #7066, .T. ) ;
#6462 = CARTESIAN_POINT ( 'NONE',  ( 14.93129073739000034, -7.087303338045999546, 320.0000000000000000 ) ) ;
#6463 = CARTESIAN_POINT ( 'NONE',  ( -0.8690672964077537088, -7.435852491287998411, -434.5070751523649051 ) ) ;
#6464 = PRODUCT_DEFINITION_CONTEXT ( 'detailed design', #5641, 'design' ) ;
#6465 = FACE_OUTER_BOUND ( 'NONE', #9587, .T. ) ;
#6466 = DIRECTION ( 'NONE',  ( -1.000000000000000000, 0.000000000000000000, 0.000000000000000000 ) ) ;
#6467 = EDGE_LOOP ( 'NONE', ( #3197, #5545, #4120, #6537 ) ) ;
#6468 = LINE ( 'NONE', #3999, #10184 ) ;
#6469 = VERTEX_POINT ( 'NONE', #7749 ) ;
#6470 = DIRECTION ( 'NONE',  ( -0.9712267471052594692, 0.000000000000000000, -0.2381566831044984178 ) ) ;
#6471 = VERTEX_POINT ( 'NONE', #290 ) ;
#6472 = CARTESIAN_POINT ( 'NONE',  ( -0.7882946689300455168, -9.499899501988618766, 315.0000000000000000 ) ) ;
#6473 = CARTESIAN_POINT ( 'NONE',  ( -15.65461689722998706, -7.260828390490999595, -302.4229045757450081 ) ) ;
#6474 = ADVANCED_FACE ( 'NONE', ( #5322 ), #2813, .F. ) ;
#6475 = DIRECTION ( 'NONE',  ( 0.000000000000000000, -1.000000000000000000, 0.000000000000000000 ) ) ;
#6476 = ADVANCED_FACE ( 'NONE', ( #7649 ), #3518, .T. ) ;
#6477 = CARTESIAN_POINT ( 'NONE',  ( -14.98500449093754483, -5.000000000000000000, -438.4247239981262396 ) ) ;
#6478 = AXIS2_PLACEMENT_3D ( 'NONE', #8132, #10598, #8992 ) ;
#6479 = PRESENTATION_STYLE_ASSIGNMENT (( #7290 ) ) ;
#6480 = ORIENTED_EDGE ( 'NONE', *, *, #7655, .F. ) ;
#6481 = CARTESIAN_POINT ( 'NONE',  ( 20.06799914428001941, -0.4075895895062001673, -302.9207377450070453 ) ) ;
#6482 = CARTESIAN_POINT ( 'NONE',  ( -41.57714395884656966, -8.000000000000000000, -366.3360218886780899 ) ) ;
#6483 = ORIENTED_EDGE ( 'NONE', *, *, #6986, .T. ) ;
#6484 = CARTESIAN_POINT ( 'NONE',  ( 8.690073206612000334, -8.569658446474999636, -314.6383426456000052 ) ) ;
#6485 = ADVANCED_FACE ( 'NONE', ( #10071 ), #1956, .F. ) ;
#6486 = CARTESIAN_POINT ( 'NONE',  ( 19.99999721801999897, 7.771189452710000131E-11, 191.0000000000000000 ) ) ;
#6487 = EDGE_LOOP ( 'NONE', ( #9108, #8131, #9080, #5494 ) ) ;
#6488 = CARTESIAN_POINT ( 'NONE',  ( 19.57080534385999471, 0.3817780055853002841, 189.9229057364800042 ) ) ;
#6489 = CIRCLE ( 'NONE', #9237, 0.9999999999999755751 ) ;
#6490 = CARTESIAN_POINT ( 'NONE',  ( 19.51240441859934194, 2.792009854621256171, 190.9999999999996589 ) ) ;
#6491 = CARTESIAN_POINT ( 'NONE',  ( 4.578722611353294170, 9.145541810471781830, -315.0000000000000568 ) ) ;
#6492 = DIRECTION ( 'NONE',  ( 0.000000000000000000, 1.000000000000000000, 0.000000000000000000 ) ) ;
#6493 = CARTESIAN_POINT ( 'NONE',  ( -16.19514236092000203, -2.730451569713999938, 315.0848619657999734 ) ) ;
#6494 = CARTESIAN_POINT ( 'NONE',  ( 0.000000000000000000, 0.000000000000000000, 0.000000000000000000 ) ) ;
#6495 = CARTESIAN_POINT ( 'NONE',  ( -10.58225433500999912, 9.538747186136999900, 320.0000000000000000 ) ) ;
#6496 = DIRECTION ( 'NONE',  ( -0.1071946444232959872, 0.000000000000000000, 0.9942380540931649024 ) ) ;
#6497 = CARTESIAN_POINT ( 'NONE',  ( -18.68762439754708637, 4.478870766961970062, 319.0000000000005116 ) ) ;
#6498 =( NAMED_UNIT ( * ) SI_UNIT ( $, .STERADIAN. ) SOLID_ANGLE_UNIT ( ) );
#6499 = CARTESIAN_POINT ( 'NONE',  ( 15.00000000000326139, -5.136019918588313243E-17, 315.0000000000001137 ) ) ;
#6500 = ORIENTED_EDGE ( 'NONE', *, *, #9162, .T. ) ;
#6501 = DIRECTION ( 'NONE',  ( 0.000000000000000000, 1.000000000000000000, 0.000000000000000000 ) ) ;
#6502 = ORIENTED_EDGE ( 'NONE', *, *, #3536, .T. ) ;
#6503 = ADVANCED_FACE ( 'NONE', ( #2713 ), #5377, .T. ) ;
#6504 = CARTESIAN_POINT ( 'NONE',  ( 3.131429216827940247E-09, -12.50000000000000000, -303.5000000000000000 ) ) ;
#6505 = CARTESIAN_POINT ( 'NONE',  ( -16.99996037728000076, 1.352916535802999941E-09, -314.9999801883000146 ) ) ;
#6506 = SHAPE_DEFINITION_REPRESENTATION ( #4412, #6273 ) ;
#6507 = CARTESIAN_POINT ( 'NONE',  ( -17.19853431800999743, 2.231396706187000145, -315.0000000000000000 ) ) ;
#6508 = CARTESIAN_POINT ( 'NONE',  ( -2.375181255485324439, -7.500000000000000888, -406.0201668106497550 ) ) ;
#6509 = CARTESIAN_POINT ( 'NONE',  ( -10.53397875998246036, -6.078358996281851390, -438.3628436008879703 ) ) ;
#6510 = CARTESIAN_POINT ( 'NONE',  ( 14.87617152917998631, 8.357511890987989744, 318.8802828394900644 ) ) ;
#6511 = CARTESIAN_POINT ( 'NONE',  ( -14.87077422265778814, -5.645617090914123004, -438.8905664445195498 ) ) ;
#6512 = CARTESIAN_POINT ( 'NONE',  ( 7.006889269069000115, 6.844138725329000472, 315.0000000000001705 ) ) ;
#6513 = DIRECTION ( 'NONE',  ( -0.02133028834981354205, 0.000000000000000000, -0.9997724835175820779 ) ) ;
#6514 = CARTESIAN_POINT ( 'NONE',  ( 19.37639879579000635, 3.420933338561999548, -317.0792622552969533 ) ) ;
#6515 = CARTESIAN_POINT ( 'NONE',  ( 9.372233899709991434, -11.04684900435999495, -316.3802825947000201 ) ) ;
#6516 = CIRCLE ( 'NONE', #9431, 4.000000000000003553 ) ;
#6517 = AXIS2_PLACEMENT_3D ( 'NONE', #8255, #3317, #6596 ) ;
#6518 = CARTESIAN_POINT ( 'NONE',  ( -19.00000000000000000, 0.000000000000000000, 319.9999999999899956 ) ) ;
#6519 = CARTESIAN_POINT ( 'NONE',  ( -0.5472160415415407986, -7.479630378048000239, -434.5564753827179061 ) ) ;
#6520 = CARTESIAN_POINT ( 'NONE',  ( -18.99997865338999858, 1.260542274312000007E-06, -316.5000000000000000 ) ) ;
#6521 = CARTESIAN_POINT ( 'NONE',  ( 11.76997148278789673, -6.834709328092291258, -315.0000000000000568 ) ) ;
#6522 = ORIENTED_EDGE ( 'NONE', *, *, #4366, .F. ) ;
#6523 = VECTOR ( 'NONE', #4871, 1000.000000000000000 ) ;
#6524 = CARTESIAN_POINT ( 'NONE',  ( -12.98706127646999953, 6.788989183774999603, -314.4963898845653603 ) ) ;
#6525 = ORIENTED_EDGE ( 'NONE', *, *, #5900, .F. ) ;
#6526 = CARTESIAN_POINT ( 'NONE',  ( 13.35645252658000004, 8.162105094466999944, -317.5000000000000000 ) ) ;
#6527 = ORIENTED_EDGE ( 'NONE', *, *, #4369, .F. ) ;
#6528 = CARTESIAN_POINT ( 'NONE',  ( 5.044863629634003921, -12.10215170741999557, -303.6197174156509391 ) ) ;
#6529 = CARTESIAN_POINT ( 'NONE',  ( 10.00000000000000000, -2.500000000000000000, -317.5000000000000000 ) ) ;
#6530 = CARTESIAN_POINT ( 'NONE',  ( 19.00000000000000000, 0.000000000000000000, 190.0000000000100044 ) ) ;
#6531 = AXIS2_PLACEMENT_3D ( 'NONE', #636, #4018, #5625 ) ;
#6532 = SURFACE_STYLE_USAGE ( .BOTH. , #939 ) ;
#6533 = AXIS2_PLACEMENT_3D ( 'NONE', #9469, #1245, #610 ) ;
#6534 = EDGE_CURVE ( 'NONE', #8216, #5301, #8657, .T. ) ;
#6535 = CARTESIAN_POINT ( 'NONE',  ( -12.66297984401999166, 9.215363186789998551, -302.4229045757450081 ) ) ;
#6536 = DIRECTION ( 'NONE',  ( 2.731587414668815965E-13, -1.000000000000000000, 2.201148506557397373E-13 ) ) ;
#6537 = ORIENTED_EDGE ( 'NONE', *, *, #7705, .T. ) ;
#6538 = CARTESIAN_POINT ( 'NONE',  ( -17.20518503178000103, -1.389427005613000032, -314.6383426456000052 ) ) ;
#6539 = CYLINDRICAL_SURFACE ( 'NONE', #2997, 4.000000000000000000 ) ;
#6540 = ORIENTED_EDGE ( 'NONE', *, *, #6263, .F. ) ;
#6541 = CARTESIAN_POINT ( 'NONE',  ( -17.30501060709000072, -4.528037784100006569, 190.0071920248299477 ) ) ;
#6542 = CARTESIAN_POINT ( 'NONE',  ( -15.61921319513150230, 7.819487029138878498, 190.9999999999996589 ) ) ;
#6543 = CARTESIAN_POINT ( 'NONE',  ( 12.16683899257771806, 6.621314373557692257, -315.0000000000001137 ) ) ;
#6544 = CARTESIAN_POINT ( 'NONE',  ( -30.87192209819000155, 2.500000000000000000, -461.0868123482000556 ) ) ;
#6545 =( BOUNDED_SURFACE ( )  B_SPLINE_SURFACE ( 3, 3, ( 
 ( #7627, #1936, #10100, #4251, #8379, #5796, #9996, #9893, #2528, #9084 ),
 ( #9137, #5045, #5204, #5904, #2637, #908, #1014, #4302, #1722, #8328 ),
 ( #5846, #10051, #965, #3334, #9941, #4197, #165, #4141, #1069, #2742 ),
 ( #7472, #1882, #115, #5100, #6009, #3441, #3390, #5153, #3497, #2582 ) ),
 .UNSPECIFIED., .F., .F., .T. ) 
 B_SPLINE_SURFACE_WITH_KNOTS ( ( 4, 4 ),
 ( 4, 1, 1, 1, 1, 1, 1, 4 ),
 ( 0.000000000000000000, 1.000000000000000000 ),
 ( 0.1266979755386999917, 0.1849192355442000057, 0.3537297013212000185, 0.5087760485612999872, 0.6503402179949999695, 0.7796319686220000156, 0.8963498434801999704, 0.9600029233005999973 ),
 .UNSPECIFIED. ) 
 GEOMETRIC_REPRESENTATION_ITEM ( )  RATIONAL_B_SPLINE_SURFACE ( (
 ( 1.237059165673999983, 1.237059165673999983, 1.237059165673999983, 1.237059165673999983, 1.237059165673999983, 1.237059165673999983, 1.237059165673999983, 1.237059165673999983, 1.237059165673999983, 1.237059165673999983),
 ( 0.9209802781085000278, 0.9209802781085000278, 0.9209802781085000278, 0.9209802781085000278, 0.9209802781085000278, 0.9209802781085000278, 0.9209802781085000278, 0.9209802781085000278, 0.9209802781085000278, 0.9209802781085000278),
 ( 0.9209802781085000278, 0.9209802781085000278, 0.9209802781085000278, 0.9209802781085000278, 0.9209802781085000278, 0.9209802781085000278, 0.9209802781085000278, 0.9209802781085000278, 0.9209802781085000278, 0.9209802781085000278),
 ( 1.237059165673999983, 1.237059165673999983, 1.237059165673999983, 1.237059165673999983, 1.237059165673999983, 1.237059165673999983, 1.237059165673999983, 1.237059165673999983, 1.237059165673999983, 1.237059165673999983) ) ) 
 REPRESENTATION_ITEM ( '' )  SURFACE ( )  );
#6546 = CARTESIAN_POINT ( 'NONE',  ( -15.39920013370999996, -4.579805981517999669, 314.6383426456000052 ) ) ;
#6547 = EDGE_CURVE ( 'NONE', #8252, #3804, #9475, .T. ) ;
#6548 = CARTESIAN_POINT ( 'NONE',  ( 17.35388116884000098, 4.663644590058999562, 320.0000000000000000 ) ) ;
#6549 = CARTESIAN_POINT ( 'NONE',  ( 11.81011838702999484, -9.634252844421009598, 320.0770942683900557 ) ) ;
#6550 = CARTESIAN_POINT ( 'NONE',  ( 10.19008647966648873, 10.76511244458322558, 319.0000000000005116 ) ) ;
#6551 = FACE_OUTER_BOUND ( 'NONE', #9372, .T. ) ;
#6552 = CARTESIAN_POINT ( 'NONE',  ( -38.59226537204000351, 2.500000000000000000, -500.7880554352000217 ) ) ;
#6553 = VERTEX_POINT ( 'NONE', #343 ) ;
#6554 = LINE ( 'NONE', #5522, #8096 ) ;
#6555 = VERTEX_POINT ( 'NONE', #6850 ) ;
#6556 = AXIS2_PLACEMENT_3D ( 'NONE', #2725, #355, #2071 ) ;
#6557 = FACE_OUTER_BOUND ( 'NONE', #5044, .T. ) ;
#6558 = DIRECTION ( 'NONE',  ( 0.000000000000000000, 1.000000000000000000, -0.000000000000000000 ) ) ;
#6559 = ITEM_DEFINED_TRANSFORMATION ( 'NONE', 'NONE', #626,  #2817 ) ;
#6560 = CARTESIAN_POINT ( 'NONE',  ( -19.86375996897344010, -1.775925728142829341, -303.4999999999996589 ) ) ;
#6561 = CARTESIAN_POINT ( 'NONE',  ( 15.71297435277999810, 3.490404421959999670, -315.0848619657999734 ) ) ;
#6562 = CIRCLE ( 'NONE', #4336, 12.00000000000001243 ) ;
#6563 = CARTESIAN_POINT ( 'NONE',  ( -19.00000000000000000, 0.000000000000000000, 190.0000000000100044 ) ) ;
#6564 = DIRECTION ( 'NONE',  ( 0.000000000000000000, 1.000000000000000000, -0.000000000000000000 ) ) ;
#6565 = AXIS2_PLACEMENT_3D ( 'NONE', #5783, #3381, #5035 ) ;
#6566 = CARTESIAN_POINT ( 'NONE',  ( 13.57573464316000056, 3.225916527208000151, -284.9999999999999432 ) ) ;
#6567 = EDGE_LOOP ( 'NONE', ( #9804, #4976 ) ) ;
#6568 = CARTESIAN_POINT ( 'NONE',  ( 16.90418428017002839, 6.814536637555997700, -317.0792622552969533 ) ) ;
#6569 = CARTESIAN_POINT ( 'NONE',  ( 7.420201433257000545, -2.500000000000000000, -419.8948508258000061 ) ) ;
#6570 = CARTESIAN_POINT ( 'NONE',  ( -11.73784133842000088, -9.026952533543999735, 320.0000000000000000 ) ) ;
#6571 = CARTESIAN_POINT ( 'NONE',  ( -1.761891692708837498, -7.351020573128999480, -434.8786339386260806 ) ) ;
#6572 = AXIS2_PLACEMENT_3D ( 'NONE', #7514, #8320, #5840 ) ;
#6573 = UNCERTAINTY_MEASURE_WITH_UNIT (LENGTH_MEASURE( 1.000000000000000082E-05 ), #5822, 'distance_accuracy_value', 'NONE');
#6574 = CARTESIAN_POINT ( 'NONE',  ( -0.6597201369859407860, -2.500000714168999938, -434.1397697187372273 ) ) ;
#6575 = CARTESIAN_POINT ( 'NONE',  ( 14.08970834377950965, -5.290460773273633954, -315.0000000000000568 ) ) ;
#6576 = VERTEX_POINT ( 'NONE', #9375 ) ;
#6577 = CARTESIAN_POINT ( 'NONE',  ( 14.57677553938589554, -5.476482737502805342, -314.5817494731896886 ) ) ;
#6578 = EDGE_LOOP ( 'NONE', ( #5148, #1916, #5130, #516 ) ) ;
#6579 = CARTESIAN_POINT ( 'NONE',  ( -0.2188334844706000260, 11.51755598686999882, -317.5000000000000000 ) ) ;
#6580 = ORIENTED_EDGE ( 'NONE', *, *, #10081, .F. ) ;
#6581 = CARTESIAN_POINT ( 'NONE',  ( 12.89386942443999295, -9.656754267509002787, -302.9207377450070453 ) ) ;
#6582 = B_SPLINE_CURVE_WITH_KNOTS ( 'NONE', 3,
 ( #1898, #4418, #129, #10013 ),
 .UNSPECIFIED., .F., .F.,
 ( 4, 4 ),
 ( 0.000000000000000000, 1.000000000000000000 ),
 .UNSPECIFIED. ) ;
#6583 = CARTESIAN_POINT ( 'NONE',  ( 10.44399617086000021, -10.22112142899999476, -317.5770954168139610 ) ) ;
#6584 = DIRECTION ( 'NONE',  ( -0.9968876850330226080, 0.000000000000000000, 0.07883491250392142546 ) ) ;
#6585 = EDGE_CURVE ( 'NONE', #2010, #6619, #6562, .T. ) ;
#6586 = CARTESIAN_POINT ( 'NONE',  ( 13.88537659940002023, 9.003549035645995957, -303.6197174156520759 ) ) ;
#6587 = PRESENTATION_LAYER_ASSIGNMENT (  '', '', ( #5209 ) ) ;
#6588 = CARTESIAN_POINT ( 'NONE',  ( -10.25126261553517537, 10.00000004282989785, 314.4997059534069308 ) ) ;
#6589 = ORIENTED_EDGE ( 'NONE', *, *, #5029, .F. ) ;
#6590 = DIRECTION ( 'NONE',  ( 1.000000000000000000, 0.000000000000000000, 0.000000000000000000 ) ) ;
#6591 = DIRECTION ( 'NONE',  ( 0.2951854283188049544, 0.000000000000000000, -0.9554399839384174475 ) ) ;
#6592 = VECTOR ( 'NONE', #3899, 1000.000000000000000 ) ;
#6593 = VERTEX_POINT ( 'NONE', #4325 ) ;
#6594 = CARTESIAN_POINT ( 'NONE',  ( -17.70739197152998656, -5.947706840970997888, 190.4207385301700128 ) ) ;
#6595 = CARTESIAN_POINT ( 'NONE',  ( -17.19853431800999743, -2.231396706187000145, -314.4944826805095772 ) ) ;
#6596 = DIRECTION ( 'NONE',  ( -0.2951854283188045658, 0.000000000000000000, 0.9554399839384175586 ) ) ;
#6597 = DIRECTION ( 'NONE',  ( 0.000000000000000000, 1.000000000000000000, 0.000000000000000000 ) ) ;
#6598 = VECTOR ( 'NONE', #650, 1000.000000000000000 ) ;
#6599 = COLOUR_RGB ( '', 0.31764706, 0.68627451, 0.89019608) ;
#6600 = EDGE_CURVE ( 'NONE', #7778, #9710, #9322, .T. ) ;
#6601 = CARTESIAN_POINT ( 'NONE',  ( 16.77957632114000219, -1.244976636274000015, 315.0848619657999734 ) ) ;
#6602 = DIRECTION ( 'NONE',  ( 0.4712473909295827323, 0.000000000000000000, -0.8820010751365675583 ) ) ;
#6603 = CARTESIAN_POINT ( 'NONE',  ( 17.84276444133998041, -4.978015457891998174, 320.0770942683900557 ) ) ;
#6604 = PLANE ( 'NONE',  #10346 ) ;
#6605 = PRESENTATION_STYLE_ASSIGNMENT (( #9025 ) ) ;
#6606 = CARTESIAN_POINT ( 'NONE',  ( 16.89608781496000134, 0.5923740909019999945, 315.0848619657999734 ) ) ;
#6607 = EDGE_LOOP ( 'NONE', ( #4725, #3169, #6502, #4015 ) ) ;
#6608 = CARTESIAN_POINT ( 'NONE',  ( 15.61921319513150053, -7.819487029138875833, 190.9999999999995737 ) ) ;
#6609 = AXIS2_PLACEMENT_3D ( 'NONE', #4435, #302, #400 ) ;
#6610 = AXIS2_PLACEMENT_3D ( 'NONE', #4091, #1462, #4743 ) ;
#6611 = ORIENTED_EDGE ( 'NONE', *, *, #762, .T. ) ;
#6612 = ORIENTED_EDGE ( 'NONE', *, *, #9605, .F. ) ;
#6613 = AXIS2_PLACEMENT_3D ( 'NONE', #625, #5501, #6308 ) ;
#6614 = EDGE_CURVE ( 'NONE', #7746, #9766, #7699, .T. ) ;
#6615 = CARTESIAN_POINT ( 'NONE',  ( -72.90663470102438737, -2.599999999999984102, -375.2168990826883714 ) ) ;
#6616 = CARTESIAN_POINT ( 'NONE',  ( 16.91975252613927694, 1.077737682115706086, 314.9999999999999432 ) ) ;
#6617 = ITEM_DEFINED_TRANSFORMATION ( 'NONE', 'NONE', #10234,  #2817 ) ;
#6618 = CARTESIAN_POINT ( 'NONE',  ( -37.57635160138833896, -8.000000000000000000, -403.2777420460153053 ) ) ;
#6619 = VERTEX_POINT ( 'NONE', #10170 ) ;
#6620 = CARTESIAN_POINT ( 'NONE',  ( -91.84750071659622961, -7.500000000000000000, -370.2190357451694922 ) ) ;
#6621 = SURFACE_STYLE_USAGE ( .BOTH. , #1022 ) ;
#6622 = CARTESIAN_POINT ( 'NONE',  ( -18.78737820286000115, 1.762683282930000095, 190.0000000000000000 ) ) ;
#6623 = EDGE_CURVE ( 'NONE', #8193, #6311, #2057, .T. ) ;
#6624 = CARTESIAN_POINT ( 'NONE',  ( -17.33381025012258903, -2.500000000000000000, -445.8348527500487535 ) ) ;
#6625 = CARTESIAN_POINT ( 'NONE',  ( 10.23467085909357976, -10.00000000050611781, 190.0000000000003695 ) ) ;
#6626 = CARTESIAN_POINT ( 'NONE',  ( -19.87640215697998158, 1.702148751976998442, -316.3802825947000201 ) ) ;
#6627 = CARTESIAN_POINT ( 'NONE',  ( -10.79636471171000167, -9.449795599854001082, 320.0000000000000000 ) ) ;
#6628 =( BOUNDED_SURFACE ( )  B_SPLINE_SURFACE ( 3, 3, ( 
 ( #8625, #1272, #3800, #8682, #8574, #7677, #10305, #472, #7090, #1120, #6111, #6159, #4402, #321, #6983, #5252, #3595, #8526, #3744, #7728, #1219, #3645, #6928, #7033, #9398, #2033, #5300, #9447, #4496, #2941, #7773, #417, #10254, #6213, #8903, #1494, #8154, #3263, #8852, #2297, #792, #6541, #1604, #8735, #9714, #10571, #4771, #9601, #4071, #3213 ),
 ( #1546, #6488, #9767, #5511, #1377, #2242, #6431, #2405, #4662, #8041, #5673, #689, #10457, #7996, #7349, #8097, #6374, #3908, #2356, #8791, #7936, #1433, #740, #8958, #634, #578, #5622, #4720, #4876, #3858, #3044, #4826, #3961, #7188, #3098, #4016, #7241, #9657, #6315, #7298, #10621, #9819, #2459, #10512, #7137, #10405, #5566, #3156, #841, #9978 ),
 ( #5777, #5080, #3533, #8203, #5946, #2620, #9233, #6811, #4337, #9122, #5882, #40, #4231, #4125, #7401, #9175, #4286, #1815, #10084, #1053, #7609, #892, #5134, #1865, #8360, #4178, #2562, #998, #3479, #258, #3315, #1651, #9925, #5727, #9016, #3372, #8413, #4927, #5830, #1756, #6594, #9876, #2513, #9068, #6700, #7558, #5026, #1704, #4977, #203 ),
 ( #6760, #10032, #8253, #8306, #947, #7505, #7451, #95, #6649, #147, #3421, #2676, #3786, #7866, #6914, #2773, #4593, #6969, #459, #1258, #2929, #9386, #10186, #10242, #6147, #8560, #7760, #9434, #4437, #4390, #9285, #6099, #4535, #1312, #2830, #7664, #3733, #402, #2020, #5287, #7020, #1970, #1206, #6863, #10292, #515, #1104, #6044, #7073, #6197 ) ),
 .UNSPECIFIED., .F., .F., .T. ) 
 B_SPLINE_SURFACE_WITH_KNOTS ( ( 4, 4 ),
 ( 4, 1, 1, 1, 1, 1, 1, 1, 1, 1, 1, 1, 1, 1, 1, 1, 1, 1, 1, 1, 1, 1, 1, 1, 1, 1, 1, 1, 1, 1, 1, 1, 1, 1, 1, 1, 1, 1, 1, 1, 1, 1, 1, 1, 1, 1, 1, 4 ),
 ( 0.000000000000000000, 1.000000000000000000 ),
 ( -0.008478179454678999930, 0.000000000000000000, 0.01942502340896999982, 0.03767429839031000149, 0.05516856733836000143, 0.07225070737889999206, 0.08921661857028999332, 0.1062419522249000020, 0.1231986756591000043, 0.1401197909732000146, 0.1574955775699000138, 0.1756558812635999889, 0.1944176066207999876, 0.2136589569993999904, 0.2335613621991999844, 0.2542018781120999882, 0.2753083038155999529, 0.2968879296931000167, 0.3196642413612000300, 0.3444503751709999673, 0.3720414184181000117, 0.4028839481288000179, 0.4370422198952000348, 0.4744802605176999810, 0.5138140658555000462, 0.5525504936030000147, 0.5886556970966999591, 0.6214671571023999697, 0.6505675624772999655, 0.6761140898808000177, 0.6991730762615999684, 0.7208971548058999979, 0.7423774111579999335, 0.7637103432859999597, 0.7842694365818000390, 0.8040102150915000578, 0.8232128915810998926, 0.8418292181656999995, 0.8596651317910000145, 0.8769212066234000069, 0.8939598742608000359, 0.9109129999441000214, 0.9278339763510999871, 0.9449158864711000305, 0.9624195949295000219, 0.9806529035300000086, 1.000000000000000000, 1.007725586608000157 ),
 .UNSPECIFIED. ) 
 GEOMETRIC_REPRESENTATION_ITEM ( )  RATIONAL_B_SPLINE_SURFACE ( (
 ( 1.236576749365999817, 1.236576749365999817, 1.236576749365999817, 1.236576749365999817, 1.236576749365999817, 1.236576749365999817, 1.236576749365999817, 1.236576749365999817, 1.236576749365999817, 1.236576749365999817, 1.236576749365999817, 1.236576749365999817, 1.236576749365999817, 1.236576749365999817, 1.236576749365999817, 1.236576749365999817, 1.236576749365999817, 1.236576749365999817, 1.236576749365999817, 1.236576749365999817, 1.236576749365999817, 1.236576749365999817, 1.236576749365999817, 1.236576749365999817, 1.236576749365999817, 1.236576749365999817, 1.236576749365999817, 1.236576749365999817, 1.236576749365999817, 1.236576749365999817, 1.236576749365999817, 1.236576749365999817, 1.236576749365999817, 1.236576749365999817, 1.236576749365999817, 1.236576749365999817, 1.236576749365999817, 1.236576749365999817, 1.236576749365999817, 1.236576749365999817, 1.236576749365999817, 1.236576749365999817, 1.236576749365999817, 1.236576749365999817, 1.236576749365999817, 1.236576749365999817, 1.236576749365999817, 1.236576749365999817, 1.236576749365999817, 1.236576749365999817),
 ( 0.9211410835446999235, 0.9211410835446999235, 0.9211410835446999235, 0.9211410835446999235, 0.9211410835446999235, 0.9211410835446999235, 0.9211410835446999235, 0.9211410835446999235, 0.9211410835446999235, 0.9211410835446999235, 0.9211410835446999235, 0.9211410835446999235, 0.9211410835446999235, 0.9211410835446999235, 0.9211410835446999235, 0.9211410835446999235, 0.9211410835446999235, 0.9211410835446999235, 0.9211410835446999235, 0.9211410835446999235, 0.9211410835446999235, 0.9211410835446999235, 0.9211410835446999235, 0.9211410835446999235, 0.9211410835446999235, 0.9211410835446999235, 0.9211410835446999235, 0.9211410835446999235, 0.9211410835446999235, 0.9211410835446999235, 0.9211410835446999235, 0.9211410835446999235, 0.9211410835446999235, 0.9211410835446999235, 0.9211410835446999235, 0.9211410835446999235, 0.9211410835446999235, 0.9211410835446999235, 0.9211410835446999235, 0.9211410835446999235, 0.9211410835446999235, 0.9211410835446999235, 0.9211410835446999235, 0.9211410835446999235, 0.9211410835446999235, 0.9211410835446999235, 0.9211410835446999235, 0.9211410835446999235, 0.9211410835446999235, 0.9211410835446999235),
 ( 0.9211410835446999235, 0.9211410835446999235, 0.9211410835446999235, 0.9211410835446999235, 0.9211410835446999235, 0.9211410835446999235, 0.9211410835446999235, 0.9211410835446999235, 0.9211410835446999235, 0.9211410835446999235, 0.9211410835446999235, 0.9211410835446999235, 0.9211410835446999235, 0.9211410835446999235, 0.9211410835446999235, 0.9211410835446999235, 0.9211410835446999235, 0.9211410835446999235, 0.9211410835446999235, 0.9211410835446999235, 0.9211410835446999235, 0.9211410835446999235, 0.9211410835446999235, 0.9211410835446999235, 0.9211410835446999235, 0.9211410835446999235, 0.9211410835446999235, 0.9211410835446999235, 0.9211410835446999235, 0.9211410835446999235, 0.9211410835446999235, 0.9211410835446999235, 0.9211410835446999235, 0.9211410835446999235, 0.9211410835446999235, 0.9211410835446999235, 0.9211410835446999235, 0.9211410835446999235, 0.9211410835446999235, 0.9211410835446999235, 0.9211410835446999235, 0.9211410835446999235, 0.9211410835446999235, 0.9211410835446999235, 0.9211410835446999235, 0.9211410835446999235, 0.9211410835446999235, 0.9211410835446999235, 0.9211410835446999235, 0.9211410835446999235),
 ( 1.236576749365999817, 1.236576749365999817, 1.236576749365999817, 1.236576749365999817, 1.236576749365999817, 1.236576749365999817, 1.236576749365999817, 1.236576749365999817, 1.236576749365999817, 1.236576749365999817, 1.236576749365999817, 1.236576749365999817, 1.236576749365999817, 1.236576749365999817, 1.236576749365999817, 1.236576749365999817, 1.236576749365999817, 1.236576749365999817, 1.236576749365999817, 1.236576749365999817, 1.236576749365999817, 1.236576749365999817, 1.236576749365999817, 1.236576749365999817, 1.236576749365999817, 1.236576749365999817, 1.236576749365999817, 1.236576749365999817, 1.236576749365999817, 1.236576749365999817, 1.236576749365999817, 1.236576749365999817, 1.236576749365999817, 1.236576749365999817, 1.236576749365999817, 1.236576749365999817, 1.236576749365999817, 1.236576749365999817, 1.236576749365999817, 1.236576749365999817, 1.236576749365999817, 1.236576749365999817, 1.236576749365999817, 1.236576749365999817, 1.236576749365999817, 1.236576749365999817, 1.236576749365999817, 1.236576749365999817, 1.236576749365999817, 1.236576749365999817) ) ) 
 REPRESENTATION_ITEM ( '' )  SURFACE ( )  );
#6629 = CARTESIAN_POINT ( 'NONE',  ( -0.1882039595137465215, -7.659278717692999727, -433.8551617668519498 ) ) ;
#6630 = DIRECTION ( 'NONE',  ( -0.9942380540931649024, 0.000000000000000000, -0.1071946444232959872 ) ) ;
#6631 = CARTESIAN_POINT ( 'NONE',  ( 1.574054099965567444, -9.469115279523553141, -315.0000000000000568 ) ) ;
#6632 = EDGE_LOOP ( 'NONE', ( #8804, #6268, #7935, #5765 ) ) ;
#6633 = COLOUR_RGB ( '', 0.40784314, 0.44705882, 0.49803922) ;
#6634 = CARTESIAN_POINT ( 'NONE',  ( 16.63862268811587697, -3.034640078201989777, -314.5459747968307056 ) ) ;
#6635 = EDGE_LOOP ( 'NONE', ( #5496, #458, #6500, #7374 ) ) ;
#6636 = CARTESIAN_POINT ( 'NONE',  ( -15.16362200326591569, -7.500000000000000000, -437.6963039377973246 ) ) ;
#6637 = ORIENTED_EDGE ( 'NONE', *, *, #373, .F. ) ;
#6638 = CARTESIAN_POINT ( 'NONE',  ( 1.673754838359998498, -12.46646309164999522, -303.6197174156509391 ) ) ;
#6639 = CARTESIAN_POINT ( 'NONE',  ( 7.796607451809997258, -10.36222334076000529, -317.4928077629770087 ) ) ;
#6640 = EDGE_CURVE ( 'NONE', #1418, #6862, #5697, .T. ) ;
#6641 = FACE_OUTER_BOUND ( 'NONE', #3247, .T. ) ;
#6642 = FILL_AREA_STYLE ('',( #8296 ) ) ;
#6643 = CARTESIAN_POINT ( 'NONE',  ( -5.561812994916270014, -7.204029759630539154, -435.9619401370908918 ) ) ;
#6644 = DIRECTION ( 'NONE',  ( 1.000000000000000000, 0.000000000000000000, 0.000000000000000000 ) ) ;
#6645 = EDGE_LOOP ( 'NONE', ( #8327, #8993, #3276, #9281 ) ) ;
#6646 = CARTESIAN_POINT ( 'NONE',  ( -17.36972170382999892, -0.04551883977364000466, -314.6383426456000052 ) ) ;
#6647 = FACE_OUTER_BOUND ( 'NONE', #3474, .T. ) ;
#6648 = VERTEX_POINT ( 'NONE', #5274 ) ;
#6649 = CARTESIAN_POINT ( 'NONE',  ( 18.17619403612001250, -5.223318733890998544, 191.1197171614399792 ) ) ;
#6650 = CARTESIAN_POINT ( 'NONE',  ( -17.19853431800999743, -2.231396706187000145, -315.0000000000001137 ) ) ;
#6651 = CARTESIAN_POINT ( 'NONE',  ( -2.000000000000000000, 3.500000000000000000, -414.5000000000000000 ) ) ;
#6652 = CARTESIAN_POINT ( 'NONE',  ( -46.74071243419621169, -9.000000000000001776, -414.3237589990241077 ) ) ;
#6653 = CARTESIAN_POINT ( 'NONE',  ( 4.478082317681002955, 12.27758592791000147, 190.4207385301700128 ) ) ;
#6654 = CARTESIAN_POINT ( 'NONE',  ( 17.35381917807999841, 0.3185724951638000402, 314.6383426456000052 ) ) ;
#6655 = DIRECTION ( 'NONE',  ( 0.2951854283188045658, 0.000000000000000000, -0.9554399839384175586 ) ) ;
#6656 = CARTESIAN_POINT ( 'NONE',  ( 18.86319819242002183, 0.4765179085981003926, 319.9928079742500131 ) ) ;
#6657 = CIRCLE ( 'NONE', #3564, 11.99999999999999289 ) ;
#6658 = CARTESIAN_POINT ( 'NONE',  ( -17.49966312145123482, 0.4461383192961264621, 314.4999388432775049 ) ) ;
#6659 = CARTESIAN_POINT ( 'NONE',  ( 12.81623431846864136, 9.609762277177448908, -303.4999999999990905 ) ) ;
#6660 = PRODUCT_DEFINITION ( 'UNKNOWN', '', #4405, #4417 ) ;
#6661 = CARTESIAN_POINT ( 'NONE',  ( 16.19514236092000203, 2.730451569713999938, 315.0848619657999734 ) ) ;
#6662 = ORIENTED_EDGE ( 'NONE', *, *, #8571, .T. ) ;
#6663 = CARTESIAN_POINT ( 'NONE',  ( -2.649465170253727297, -12.40913386102118210, 190.9999999999995737 ) ) ;
#6664 = VERTEX_POINT ( 'NONE', #9422 ) ;
#6665 = LINE ( 'NONE', #4354, #4772 ) ;
#6666 = CARTESIAN_POINT ( 'NONE',  ( 5.850395566949658566, 8.918560297860793185, 315.0000000000000000 ) ) ;
#6667 = CYLINDRICAL_SURFACE ( 'NONE', #8744, 0.5000000000000066613 ) ;
#6668 = EDGE_LOOP ( 'NONE', ( #4835, #291 ) ) ;
#6669 = ORIENTED_EDGE ( 'NONE', *, *, #2264, .T. ) ;
#6670 = LINE ( 'NONE', #3651, #9518 ) ;
#6671 = DIRECTION ( 'NONE',  ( 0.000000000000000000, -1.000000000000000000, 0.000000000000000000 ) ) ;
#6672 = CARTESIAN_POINT ( 'NONE',  ( 11.56195786956000049, 9.110631795823000090, 190.0000000000000000 ) ) ;
#6673 = CARTESIAN_POINT ( 'NONE',  ( -11.28781796570999951, 4.951468039558000633, 315.0000000000001705 ) ) ;
#6674 = CARTESIAN_POINT ( 'NONE',  ( -24.00000000000000000, 2.500000000000000000, -380.4979246178999688 ) ) ;
#6675 = CARTESIAN_POINT ( 'NONE',  ( 6.467159262072997628, 11.83367582535999141, -316.3802825947000201 ) ) ;
#6676 = CARTESIAN_POINT ( 'NONE',  ( -72.90663470102438737, -12.50000000000000000, -371.7168990826883714 ) ) ;
#6677 = EDGE_CURVE ( 'NONE', #6416, #9387, #4522, .T. ) ;
#6678 = CARTESIAN_POINT ( 'NONE',  ( 8.494641066709883503, -5.769732973146090238, -525.6795250154979158 ) ) ;
#6679 = CARTESIAN_POINT ( 'NONE',  ( 16.99996037728000076, -1.352915083302999933E-09, -314.9999801883000146 ) ) ;
#6680 = ADVANCED_FACE ( 'NONE', ( #9684 ), #8814, .F. ) ;
#6681 = CARTESIAN_POINT ( 'NONE',  ( 10.54249803899487503, -7.451732067202642362, -315.0000000000000568 ) ) ;
#6682 = VERTEX_POINT ( 'NONE', #4900 ) ;
#6683 = CARTESIAN_POINT ( 'NONE',  ( 15.54345086749722427, -4.503564883714266998, -314.5712070352258820 ) ) ;
#6684 = VERTEX_POINT ( 'NONE', #9 ) ;
#6685 = CARTESIAN_POINT ( 'NONE',  ( 18.86945318303000008, 1.615078380336999908, -317.5000000000470095 ) ) ;
#6686 = VERTEX_POINT ( 'NONE', #6624 ) ;
#6687 = CARTESIAN_POINT ( 'NONE',  ( 12.85477847496998827, -9.582024189157998251, -303.6197174156520759 ) ) ;
#6688 = VECTOR ( 'NONE', #5748, 1000.000000000000000 ) ;
#6689 = VECTOR ( 'NONE', #4484, 1000.000000000000000 ) ;
#6690 = DIRECTION ( 'NONE',  ( 0.9620620651437388204, -2.527616691482515415E-15, -0.2728306852451987674 ) ) ;
#6691 = CYLINDRICAL_SURFACE ( 'NONE', #8313, 14.99999999999999112 ) ;
#6692 = AXIS2_PLACEMENT_3D ( 'NONE', #9896, #5156, #1670 ) ;
#6693 = CARTESIAN_POINT ( 'NONE',  ( -13.97988708520999701, 9.045087908074000538, -302.9207377450070453 ) ) ;
#6694 = EDGE_CURVE ( 'NONE', #9268, #10547, #9289, .T. ) ;
#6695 = CARTESIAN_POINT ( 'NONE',  ( 2.381287022736665303E-07, -10.00000000000000000, 314.4997059534069308 ) ) ;
#6696 = ORIENTED_EDGE ( 'NONE', *, *, #6614, .F. ) ;
#6697 = CARTESIAN_POINT ( 'NONE',  ( -0.5580839194863698172, -7.499999952522999891, -434.2754015600911544 ) ) ;
#6698 = CARTESIAN_POINT ( 'NONE',  ( -17.63021146919999893, 4.299866645372000029, -302.4999999999969873 ) ) ;
#6699 = ORIENTED_EDGE ( 'NONE', *, *, #1199, .T. ) ;
#6700 = CARTESIAN_POINT ( 'NONE',  ( -19.58491037614999897, -2.818636756334000903, 190.4207385301700128 ) ) ;
#6701 = CARTESIAN_POINT ( 'NONE',  ( -87.43676691142619006, -2.500000000000000000, -348.7659131681800773 ) ) ;
#6702 = CARTESIAN_POINT ( 'NONE',  ( 19.38368284813939013, -7.500000000000000000, -515.5999187775453265 ) ) ;
#6703 = B_SPLINE_CURVE_WITH_KNOTS ( 'NONE', 3,
 ( #4503, #7780, #2090, #5357, #4077, #3967, #798, #6548, #8799, #3105, #5517, #4561, #1440, #4728, #6321, #642, #8857, #4024, #8967, #10576, #847, #9022, #7248, #8001, #7355, #3218, #1499, #3270, #9773, #5575, #7304, #6495, #5627, #4831, #2414, #4781, #3918, #9609, #3163, #1610, #1658, #8102, #6438, #9662, #7195, #744, #9827, #5680 ),
 .UNSPECIFIED., .F., .F.,
 ( 4, 1, 1, 1, 1, 1, 1, 1, 1, 1, 1, 1, 1, 1, 1, 1, 1, 1, 1, 1, 1, 1, 1, 1, 1, 1, 1, 1, 1, 1, 1, 1, 1, 1, 1, 1, 1, 1, 1, 1, 1, 1, 1, 1, 1, 4 ),
 ( 0.000000000000000000, 0.02222222222221999915, 0.04444444444443999831, 0.06666666666666999641, 0.08888888888889000250, 0.1111111111111000027, 0.1333333333332999970, 0.1555555555555999947, 0.1777777777777999890, 0.2000000000000000111, 0.2222222222222000054, 0.2444444444443999997, 0.2666666666666999697, 0.2888888888889000195, 0.3111111111111000138, 0.3333333333333000081, 0.3555555555556000336, 0.3777777777777999724, 0.4000000000000000222, 0.4222222222221999610, 0.4444444444444000109, 0.4666666666666999808, 0.4888888888889000306, 0.5111111111110999694, 0.5333333333333000192, 0.5555555555555999891, 0.5777777777778000390, 0.5999999999999999778, 0.6222222222222000276, 0.6444444444443999664, 0.6666666666667000474, 0.6888888888888999862, 0.7111111111111000360, 0.7333333333333000859, 0.7555555555556000558, 0.7777777777777999946, 0.8000000000000000444, 0.8222222222221999832, 0.8444444444443999220, 0.8666666666667000030, 0.8888888888888999418, 0.9111111111110999916, 0.9333333333333000414, 0.9555555555556000114, 0.9777777777778000612, 1.000000000000000000 ),
 .UNSPECIFIED. ) ;
#6704 = CARTESIAN_POINT ( 'NONE',  ( -38.85901494634669007, -7.500000000001000977, -386.6556615250812570 ) ) ;
#6705 = CARTESIAN_POINT ( 'NONE',  ( -12.19509678855998835, 10.00267306739999640, 190.4207385301700128 ) ) ;
#6706 = CIRCLE ( 'NONE', #1538, 20.50000098869999832 ) ;
#6707 = CARTESIAN_POINT ( 'NONE',  ( 12.17979804859000126, -7.053762231097000068, 314.6383426456000052 ) ) ;
#6708 = CARTESIAN_POINT ( 'NONE',  ( -2.000000000000000000, 4.200000000000000178, -409.5000000000000000 ) ) ;
#6709 = CARTESIAN_POINT ( 'NONE',  ( -18.35207017878000357, -4.220106527025000887, 320.0770942683900557 ) ) ;
#6710 = DIRECTION ( 'NONE',  ( 0.1071946444232958900, 0.000000000000000000, -0.9942380540931649024 ) ) ;
#6711 = CARTESIAN_POINT ( 'NONE',  ( 9.314945463565894812, 11.07333627012143573, -303.4999999999990905 ) ) ;
#6712 = CARTESIAN_POINT ( 'NONE',  ( 10.32396869588999877, 7.471487098147999717, 315.0848619657999734 ) ) ;
#6713 = EDGE_CURVE ( 'NONE', #8834, #4003, #2064, .T. ) ;
#6714 = ORIENTED_EDGE ( 'NONE', *, *, #1595, .T. ) ;
#6715 = CARTESIAN_POINT ( 'NONE',  ( -13.93599793909949369, -8.976999749472309276, 190.9999999999995737 ) ) ;
#6716 = VERTEX_POINT ( 'NONE', #66 ) ;
#6717 = CARTESIAN_POINT ( 'NONE',  ( 19.78455541125000750, 1.880268586931002073, 318.8802828394900644 ) ) ;
#6718 = VERTEX_POINT ( 'NONE', #4999 ) ;
#6719 = ORIENTED_EDGE ( 'NONE', *, *, #2398, .F. ) ;
#6720 = CARTESIAN_POINT ( 'NONE',  ( -76.59645255500944927, -7.500000000000000888, -359.7738992834581495 ) ) ;
#6721 = CARTESIAN_POINT ( 'NONE',  ( -13.67632236045006167, 5.618997091738346050, 315.0000000000000000 ) ) ;
#6722 = CONTEXT_DEPENDENT_SHAPE_REPRESENTATION ( #5991, #1149 ) ;
#6723 = CARTESIAN_POINT ( 'NONE',  ( -13.57573464316000056, -3.225916527208000151, -285.0000000000000000 ) ) ;
#6724 = ORIENTED_EDGE ( 'NONE', *, *, #1199, .F. ) ;
#6725 = CARTESIAN_POINT ( 'NONE',  ( 14.35075321877000043, -7.519064610420000072, -302.5000000000000000 ) ) ;
#6726 = SURFACE_STYLE_FILL_AREA ( #3448 ) ;
#6727 = ADVANCED_FACE ( 'NONE', ( #7531 ), #8280, .F. ) ;
#6728 = CARTESIAN_POINT ( 'NONE',  ( 10.60011422839999895, 9.531420659438001763, 190.0000000000000000 ) ) ;
#6729 = CARTESIAN_POINT ( 'NONE',  ( 9.425149342036858613, -8.435515065082231700, 314.4999430218500720 ) ) ;
#6730 = DIRECTION ( 'NONE',  ( 0.000000000000000000, 1.000000000000000000, 0.000000000000000000 ) ) ;
#6732 = DIRECTION ( 'NONE',  ( 0.000000000000000000, -1.000000000000000000, 0.000000000000000000 ) ) ;
#6731 = CIRCLE ( 'NONE', #7583, 1.999999999999980238 ) ;
#6733 = DIRECTION ( 'NONE',  ( 0.000000000000000000, 1.000000000000000000, 0.000000000000000000 ) ) ;
#6734 = EDGE_CURVE ( 'NONE', #3477, #1984, #2419, .T. ) ;
#6735 = CARTESIAN_POINT ( 'NONE',  ( 18.99998145310000197, -0.3132853329045000024, 319.9999999999899956 ) ) ;
#6736 = EDGE_CURVE ( 'NONE', #7240, #8504, #4818, .T. ) ;
#6737 = CARTESIAN_POINT ( 'NONE',  ( -37.72923359849013281, -8.000000000000000000, -403.2942251520989316 ) ) ;
#6738 = AXIS2_PLACEMENT_3D ( 'NONE', #10019, #1191, #3722 ) ;
#6739 = CARTESIAN_POINT ( 'NONE',  ( 17.50000000000000000, 0.7437989020623000380, -315.0000000000000000 ) ) ;
#6740 = CARTESIAN_POINT ( 'NONE',  ( 15.46045765806406891, -3.925441769934805869, -315.0000000000001137 ) ) ;
#6741 = AXIS2_PLACEMENT_3D ( 'NONE', #4293, #5999, #4240 ) ;
#6742 = ORIENTED_EDGE ( 'NONE', *, *, #9491, .T. ) ;
#6743 = CARTESIAN_POINT ( 'NONE',  ( 17.50000000000107292, 0.7437989020622546299, -315.0000000000001137 ) ) ;
#6744 = DIRECTION ( 'NONE',  ( 0.2756373558169616378, 0.000000000000000000, -0.9612616959383295523 ) ) ;
#6745 = EDGE_LOOP ( 'NONE', ( #8930, #10342, #1493, #2177 ) ) ;
#6746 = CARTESIAN_POINT ( 'NONE',  ( -39.23786858994942151, -9.633703999999999823, -387.8670522075712483 ) ) ;
#6747 = VERTEX_POINT ( 'NONE', #4950 ) ;
#6748 = CARTESIAN_POINT ( 'NONE',  ( 18.63306024686997375, -4.746768565380000027, -302.9207377450070453 ) ) ;
#6749 = CARTESIAN_POINT ( 'NONE',  ( -13.31532601970998897, -8.047348965112000485, -317.4928077629770087 ) ) ;
#6750 = ADVANCED_FACE ( 'NONE', ( #2485 ), #8540, .F. ) ;
#6751 = VECTOR ( 'NONE', #7808, 1000.000000000000000 ) ;
#6752 = CARTESIAN_POINT ( 'NONE',  ( 17.50000000000000000, 0.000000000000000000, -314.4999343908002629 ) ) ;
#6753 = CARTESIAN_POINT ( 'NONE',  ( 0.000000000000000000, 0.000000000000000000, 0.000000000000000000 ) ) ;
#6754 = CARTESIAN_POINT ( 'NONE',  ( -12.85477847496998827, 9.582024189157998251, -303.6197174156520759 ) ) ;
#6755 = CARTESIAN_POINT ( 'NONE',  ( -100.2082379103963063, -7.500000000000000000, -339.7166298527751565 ) ) ;
#6756 = ORIENTED_EDGE ( 'NONE', *, *, #8507, .T. ) ;
#6757 = CARTESIAN_POINT ( 'NONE',  ( -46.74071243419000155, 2.500000000000000000, -414.3237589990000629 ) ) ;
#6758 = CARTESIAN_POINT ( 'NONE',  ( -82.18980308971114823, -2.366295999999999733, -388.2946789300659134 ) ) ;
#6759 = VERTEX_POINT ( 'NONE', #6113 ) ;
#6760 = CARTESIAN_POINT ( 'NONE',  ( 19.97280825118999914, 0.5561396363675005228, 191.1197171614399792 ) ) ;
#6761 = FACE_OUTER_BOUND ( 'NONE', #2122, .T. ) ;
#6762 = DIRECTION ( 'NONE',  ( -0.9712267471052594692, 0.000000000000000000, -0.2381566831044984178 ) ) ;
#6763 = CARTESIAN_POINT ( 'NONE',  ( -20.00511239988002998, 0.1020359997562000631, 191.1197171614399792 ) ) ;
#6764 = AXIS2_PLACEMENT_3D ( 'NONE', #9123, #5027, #3480 ) ;
#6765 = CARTESIAN_POINT ( 'NONE',  ( 16.97404422732000029, -2.118410180888999683, 314.6383426456000052 ) ) ;
#6766 =( NAMED_UNIT ( * ) PLANE_ANGLE_UNIT ( ) SI_UNIT ( $, .RADIAN. ) );
#6767 = DIRECTION ( 'NONE',  ( 1.000000000000000000, 0.000000000000000000, 0.000000000000000000 ) ) ;
#6768 = CARTESIAN_POINT ( 'NONE',  ( 10.81481884307000207, -10.07000335707000538, 320.0770942683900557 ) ) ;
#6769 = CARTESIAN_POINT ( 'NONE',  ( -77.27620995684556249, -2.500000000000000000, -327.4641976886060206 ) ) ;
#6770 = CARTESIAN_POINT ( 'NONE',  ( -5.046018101664360600, 12.10925368423180437, -303.5000000000000000 ) ) ;
#6771 = CARTESIAN_POINT ( 'NONE',  ( 16.98808798087999961, 1.334629195702000004, 314.8616023057000461 ) ) ;
#6772 = ORIENTED_EDGE ( 'NONE', *, *, #10284, .T. ) ;
#6773 = LINE ( 'NONE', #8425, #8436 ) ;
#6774 = CARTESIAN_POINT ( 'NONE',  ( -2.578726422179000721, 12.49238522902999726, 319.5792614743400009 ) ) ;
#6775 = VECTOR ( 'NONE', #2852, 1000.000000000000000 ) ;
#6776 = CLOSED_SHELL ( 'NONE', ( #1239, #5266, #7292, #9838, #7012, #5605, #1667, #4122, #3803, #8696, #2828, #10609, #8704, #7806, #2504, #6476, #5009, #2120, #3397, #1801, #5328, #2246, #5015, #2078, #3204, #5885, #1277 ) ) ;
#6777 = CARTESIAN_POINT ( 'NONE',  ( 19.38368284813939013, -2.500000000000000000, -515.5999187775453265 ) ) ;
#6778 = CARTESIAN_POINT ( 'NONE',  ( 8.666088325696231109, 8.161304309888411268, 315.0000000000000568 ) ) ;
#6779 = CONTEXT_DEPENDENT_SHAPE_REPRESENTATION ( #559, #9311 ) ;
#6780 = DIRECTION ( 'NONE',  ( -0.9712267471052594692, 0.000000000000000000, -0.2381566831044984178 ) ) ;
#6781 = VECTOR ( 'NONE', #4590, 1000.000000000000000 ) ;
#6782 = VECTOR ( 'NONE', #2588, 1000.000000000000000 ) ;
#6783 = ORIENTED_EDGE ( 'NONE', *, *, #8962, .F. ) ;
#6784 = CARTESIAN_POINT ( 'NONE',  ( 13.37992741786000117, -8.147955808703001068, -302.5000000000000000 ) ) ;
#6785 = CARTESIAN_POINT ( 'NONE',  ( 0.000000000000000000, 0.000000000000000000, -285.0000000000000000 ) ) ;
#6786 = CARTESIAN_POINT ( 'NONE',  ( 18.95710617844000012, 0.9155000425601000913, 190.0000000000000000 ) ) ;
#6787 = CARTESIAN_POINT ( 'NONE',  ( -15.60727917143683463, 3.742131089528406118, -315.0000000000000568 ) ) ;
#6788 = CARTESIAN_POINT ( 'NONE',  ( -14.79012398734008293, 1.483731117706880154, 315.0000000000001705 ) ) ;
#6789 = DIRECTION ( 'NONE',  ( -0.7426245373610013134, 0.000000000000000000, 0.6697079934638370258 ) ) ;
#6790 = CYLINDRICAL_SURFACE ( 'NONE', #4064, 11.00000000000000000 ) ;
#6791 = PRESENTATION_LAYER_ASSIGNMENT (  '', '', ( #6089 ) ) ;
#6792 = CARTESIAN_POINT ( 'NONE',  ( 18.53283357168000123, -2.549981878952999992, 320.0000000000000000 ) ) ;
#6793 = CARTESIAN_POINT ( 'NONE',  ( -46.99043262408034138, -7.500000000000000888, -367.5208101669372240 ) ) ;
#6794 = DIRECTION ( 'NONE',  ( 0.2728306852451984343, 0.000000000000000000, 0.9620620651437388204 ) ) ;
#6795 = EDGE_LOOP ( 'NONE', ( #6714, #4218 ) ) ;
#6796 = CARTESIAN_POINT ( 'NONE',  ( 18.85507443398999428, 0.7700411122678003650, 319.9928079742500131 ) ) ;
#6797 = CARTESIAN_POINT ( 'NONE',  ( 12.86685525668169561, -9.583295652123236863, -316.5000000000004547 ) ) ;
#6798 = ORIENTED_EDGE ( 'NONE', *, *, #4052, .T. ) ;
#6799 = DIRECTION ( 'NONE',  ( 1.000000000000000000, 0.000000000000000000, 0.000000000000000000 ) ) ;
#6800 = EDGE_LOOP ( 'NONE', ( #7458, #5726, #1877, #2517 ) ) ;
#6801 = CARTESIAN_POINT ( 'NONE',  ( -12.34703828426001770, 8.590819132751997600, -317.4928077629770087 ) ) ;
#6802 = CARTESIAN_POINT ( 'NONE',  ( 5.251781279335003383, -11.64703610505998910, -317.5770954168139610 ) ) ;
#6803 = CARTESIAN_POINT ( 'NONE',  ( -16.80445917461999983, 3.015803745947999825, -314.4150829855000211 ) ) ;
#6804 = PRESENTATION_LAYER_ASSIGNMENT (  '', '', ( #2000 ) ) ;
#6805 = CARTESIAN_POINT ( 'NONE',  ( -17.74191744551998795, 5.793625128177000150, -303.6197174156520759 ) ) ;
#6806 = ORIENTED_EDGE ( 'NONE', *, *, #6585, .T. ) ;
#6807 = CARTESIAN_POINT ( 'NONE',  ( 18.95640219669000004, -0.9217981998336000071, 190.0000000000000000 ) ) ;
#6808 = ADVANCED_FACE ( 'NONE', ( #7092 ), #7562, .T. ) ;
#6809 = DIRECTION ( 'NONE',  ( 0.000000000000000000, 0.000000000000000000, -1.000000000000000000 ) ) ;
#6810 = ORIENTED_EDGE ( 'NONE', *, *, #8293, .T. ) ;
#6811 = CARTESIAN_POINT ( 'NONE',  ( 18.75323799499002675, -4.519634888734000100, 190.4207385301700128 ) ) ;
#6812 = LINE ( 'NONE', #10085, #4870 ) ;
#6813 = CARTESIAN_POINT ( 'NONE',  ( 17.62731894649998665, -4.091366980619998373, -302.5071922382879279 ) ) ;
#6814 = EDGE_CURVE ( 'NONE', #886, #7746, #6010, .T. ) ;
#6815 = CARTESIAN_POINT ( 'NONE',  ( -14.87873868498998498, 8.458320990069003287, 190.4207385301700128 ) ) ;
#6816 = TOROIDAL_SURFACE ( 'NONE', #8183, 15.50000000000000000, 0.5000000000000000000 ) ;
#6817 = CARTESIAN_POINT ( 'NONE',  ( 13.62823431091000081, -6.408810695481999886, 314.4150829855000211 ) ) ;
#6818 = SURFACE_SIDE_STYLE ('',( #3486 ) ) ;
#6819 = EDGE_CURVE ( 'NONE', #199, #7857, #8932, .T. ) ;
#6820 = DIRECTION ( 'NONE',  ( 1.000000000000000000, 0.000000000000000000, 0.000000000000000000 ) ) ;
#6821 = CARTESIAN_POINT ( 'NONE',  ( -9.099181536070998888, -11.22222323403999766, 319.5792614743400009 ) ) ;
#6822 = CARTESIAN_POINT ( 'NONE',  ( -16.24773437005479693, 3.756014688789979683, 314.4999406160052331 ) ) ;
#6823 = DIRECTION ( 'NONE',  ( 0.000000000000000000, 1.000000000000000000, 0.000000000000000000 ) ) ;
#6824 = EDGE_CURVE ( 'NONE', #8080, #3828, #10060, .T. ) ;
#6825 = CARTESIAN_POINT ( 'NONE',  ( 16.25556153634000367, 3.885850782616000032, 314.4150829855000211 ) ) ;
#6826 = EDGE_LOOP ( 'NONE', ( #7475, #10185, #6347, #6637 ) ) ;
#6827 = CARTESIAN_POINT ( 'NONE',  ( 9.013443235573840084, -11.16848941897282899, 190.9999999999995737 ) ) ;
#6828 = CARTESIAN_POINT ( 'NONE',  ( 20.08924610253000509, 0.07535283344304002928, 319.5792614743400009 ) ) ;
#6829 = DIRECTION ( 'NONE',  ( 0.000000000000000000, 0.000000000000000000, -1.000000000000000000 ) ) ;
#6830 = AXIS2_PLACEMENT_3D ( 'NONE', #920, #5216, #8493 ) ;
#6831 = CARTESIAN_POINT ( 'NONE',  ( 4.252796533868254514, 9.197585063050969012, 315.0000000000000568 ) ) ;
#6832 = CARTESIAN_POINT ( 'NONE',  ( -15.00000000000071587, -0.4945770392355663403, -284.9999999999999432 ) ) ;
#6833 = VERTEX_POINT ( 'NONE', #6161 ) ;
#6834 = DIRECTION ( 'NONE',  ( 1.000000000000000000, 0.000000000000000000, 0.000000000000000000 ) ) ;
#6835 = DIRECTION ( 'NONE',  ( 0.4712473909295827323, 0.000000000000000000, -0.8820010751365675583 ) ) ;
#6836 = ADVANCED_FACE ( 'NONE', ( #9450 ), #6271, .T. ) ;
#6837 = CARTESIAN_POINT ( 'NONE',  ( 12.50247260085999912, 8.641513563414997989, 190.0000000000000000 ) ) ;
#6838 = DIRECTION ( 'NONE',  ( 0.9554399839384175586, 0.000000000000000000, 0.2951854283188048989 ) ) ;
#6839 = CARTESIAN_POINT ( 'NONE',  ( -14.93050028969001808, 6.935770771621001529, 190.0071920248299477 ) ) ;
#6840 = VECTOR ( 'NONE', #5246, 1000.000000000000000 ) ;
#6841 = CARTESIAN_POINT ( 'NONE',  ( -39.23786858994942151, -7.500000000000000888, -387.8670522075712483 ) ) ;
#6842 = CYLINDRICAL_SURFACE ( 'NONE', #1324, 3.500000000000003109 ) ;
#6843 = CYLINDRICAL_SURFACE ( 'NONE', #2544, 0.5000000000000004441 ) ;
#6844 = CARTESIAN_POINT ( 'NONE',  ( -69.81963093799060971, -2.500000000000000000, -370.0675332144908793 ) ) ;
#6845 = EDGE_LOOP ( 'NONE', ( #4973, #2979, #6719, #3249 ) ) ;
#6846 = CARTESIAN_POINT ( 'NONE',  ( -119.6503683519543983, -2.500000000000000000, -299.0840866897705155 ) ) ;
#6847 = CARTESIAN_POINT ( 'NONE',  ( -18.54292857607040901, -4.743390938996658868, -316.5000000000004547 ) ) ;
#6848 = ORIENTED_EDGE ( 'NONE', *, *, #7668, .F. ) ;
#6849 = EDGE_CURVE ( 'NONE', #4552, #4872, #7050, .T. ) ;
#6850 = CARTESIAN_POINT ( 'NONE',  ( -0.3140675329811673522, -8.000000000000000000, -361.6501536237392429 ) ) ;
#6851 = ORIENTED_EDGE ( 'NONE', *, *, #2921, .T. ) ;
#6852 = CARTESIAN_POINT ( 'NONE',  ( -5.133129775586001031, 10.95790389472999316, -317.4928077629770087 ) ) ;
#6853 = CARTESIAN_POINT ( 'NONE',  ( -19.37639879579000635, -3.420933338561999548, -317.0792622552969533 ) ) ;
#6854 = CARTESIAN_POINT ( 'NONE',  ( -19.00000000000000000, 0.000000000000000000, 319.9999999999899956 ) ) ;
#6855 = DIRECTION ( 'NONE',  ( 0.000000000000000000, 0.000000000000000000, -1.000000000000000000 ) ) ;
#6856 = CARTESIAN_POINT ( 'NONE',  ( -85.25464975288055314, -2.500000000000000000, -378.3143625557585779 ) ) ;
#6857 = ORIENTED_EDGE ( 'NONE', *, *, #7743, .T. ) ;
#6858 = CARTESIAN_POINT ( 'NONE',  ( -4.353497780899999725, -11.20674699699000065, 190.0000000000000000 ) ) ;
#6859 = AXIS2_PLACEMENT_3D ( 'NONE', #691, #8961, #2245 ) ;
#6860 = CARTESIAN_POINT ( 'NONE',  ( 2.381287040813000348E-07, -10.00000001404999850, 190.0000000000000000 ) ) ;
#6861 = EDGE_CURVE ( 'NONE', #1530, #5334, #10307, .T. ) ;
#6862 = VERTEX_POINT ( 'NONE', #476 ) ;
#6863 = CARTESIAN_POINT ( 'NONE',  ( -19.14223954934999483, -3.638712114223002558, 191.1197171614399792 ) ) ;
#6864 = EDGE_LOOP ( 'NONE', ( #7281, #9780, #7756, #2636 ) ) ;
#6865 = CARTESIAN_POINT ( 'NONE',  ( -16.40981772118269788, -2.462276419762760682, 314.9999999999999432 ) ) ;
#6866 = CARTESIAN_POINT ( 'NONE',  ( -7.736889024074004695, -10.37866566675000435, -302.5071922382879279 ) ) ;
#6867 = CARTESIAN_POINT ( 'NONE',  ( -19.98387668437998954, -0.4031290841194005714, 191.1197171614399792 ) ) ;
#6868 = AXIS2_PLACEMENT_3D ( 'NONE', #7435, #10601, #72 ) ;
#6869 = ADVANCED_FACE ( 'NONE', ( #3699, #9550 ), #6216, .T. ) ;
#6870 = LINE ( 'NONE', #8617, #5448 ) ;
#6871 = FILL_AREA_STYLE ('',( #410 ) ) ;
#6872 = EDGE_CURVE ( 'NONE', #5811, #5378, #580, .T. ) ;
#6873 = CARTESIAN_POINT ( 'NONE',  ( 18.87259549714001139, -0.3457787829170000937, -302.5071922382879279 ) ) ;
#6874 = CARTESIAN_POINT ( 'NONE',  ( -4.941041030666997180, -12.20591504665998350, 319.5792614743400009 ) ) ;
#6875 = DIRECTION ( 'NONE',  ( -0.1167903181061911294, 0.000000000000000000, 0.9931565947002791717 ) ) ;
#6876 = CARTESIAN_POINT ( 'NONE',  ( -1.399029207469000058, 9.644928263550999858, 314.8616023057000461 ) ) ;
#6877 = ORIENTED_EDGE ( 'NONE', *, *, #6967, .T. ) ;
#6878 = CARTESIAN_POINT ( 'NONE',  ( -17.64879272652969888, -5.897502810282468921, 190.9999999999995737 ) ) ;
#6879 = ORIENTED_EDGE ( 'NONE', *, *, #1682, .T. ) ;
#6880 = CARTESIAN_POINT ( 'NONE',  ( 18.27279225368999249, 5.234253896328004529, 319.5792614743400009 ) ) ;
#6881 = CIRCLE ( 'NONE', #179, 0.5000000000000004441 ) ;
#6882 = EDGE_CURVE ( 'NONE', #4012, #8127, #2845, .T. ) ;
#6883 = CARTESIAN_POINT ( 'NONE',  ( -72.90663470102438737, 7.399494936611693774, -375.2168990826883714 ) ) ;
#6884 = AXIS2_PLACEMENT_3D ( 'NONE', #1607, #7243, #10514 ) ;
#6885 = CARTESIAN_POINT ( 'NONE',  ( -1.669669261120717341, 9.454727574740482865, 315.0000000000000568 ) ) ;
#6886 = CARTESIAN_POINT ( 'NONE',  ( 0.000000000000000000, -10.00000000000000000, 315.0000000000000000 ) ) ;
#6887 = VECTOR ( 'NONE', #1351, 1000.000000000000000 ) ;
#6888 = FACE_OUTER_BOUND ( 'NONE', #877, .T. ) ;
#6889 = CARTESIAN_POINT ( 'NONE',  ( -46.74071243419621169, -8.000000000000000000, -414.3237589990241077 ) ) ;
#6890 = CARTESIAN_POINT ( 'NONE',  ( 18.20814976352000158, 3.283820199526999772, 190.0000000000000000 ) ) ;
#6891 = CARTESIAN_POINT ( 'NONE',  ( 14.91207369124052740, -5.270756709766473591, 314.4999413757460047 ) ) ;
#6892 = CARTESIAN_POINT ( 'NONE',  ( -11.67891759455000056, 8.922363378240000031, 190.0071920248299477 ) ) ;
#6893 = CARTESIAN_POINT ( 'NONE',  ( 14.00000000000000000, -2.500000000000000000, -272.5000000000000000 ) ) ;
#6894 =( BOUNDED_CURVE ( )  B_SPLINE_CURVE ( 3, ( #6934, #1333, #5206, #8636, #4612, #8580, #6886 ),
 .UNSPECIFIED., .F., .T. ) 
 B_SPLINE_CURVE_WITH_KNOTS ( ( 4, 3, 4 ),
 ( 0.000000000000000000, 0.5000000000000000000, 1.000000000000000000 ),
 .UNSPECIFIED. ) 
 CURVE ( )  GEOMETRIC_REPRESENTATION_ITEM ( )  RATIONAL_B_SPLINE_CURVE ( ( 1.000000000000000000, 0.8047378516590519837, 0.8047378516590519837, 1.000000000000000000, 0.8047378516590519837, 0.8047378516590519837, 1.000000000000000000 ) ) 
 REPRESENTATION_ITEM ( '' )  );
#6895 = CARTESIAN_POINT ( 'NONE',  ( -18.32252861763999974, -3.123808493131999597, -317.4999999999870397 ) ) ;
#6896 = CYLINDRICAL_SURFACE ( 'NONE', #5281, 0.5000000000000172085 ) ;
#6897 = CARTESIAN_POINT ( 'NONE',  ( 13.95695539824072640, -5.398716172439862682, 315.0000000000000568 ) ) ;
#6898 = CARTESIAN_POINT ( 'NONE',  ( -13.50042001888999899, 6.225262767767000049, -314.6383426456000052 ) ) ;
#6899 = ORIENTED_EDGE ( 'NONE', *, *, #8242, .F. ) ;
#6900 = CARTESIAN_POINT ( 'NONE',  ( -37.62994892356022092, -9.000000000000001776, -402.7806230189644339 ) ) ;
#6901 = CARTESIAN_POINT ( 'NONE',  ( 15.96117728870900088, -7.554047240424474730, -316.5000000000004547 ) ) ;
#6902 = DIRECTION ( 'NONE',  ( 0.000000000000000000, -1.000000000000000000, 0.000000000000000000 ) ) ;
#6903 = VERTEX_POINT ( 'NONE', #1026 ) ;
#6904 = CARTESIAN_POINT ( 'NONE',  ( -1.873948611771682149, -12.00000000000000000, -349.2478646809681777 ) ) ;
#6905 = CARTESIAN_POINT ( 'NONE',  ( 16.93681971163998057, -6.782628217974004059, -317.0792622552969533 ) ) ;
#6906 = PRODUCT_DEFINITION_SHAPE ( 'NONE', 'NONE',  #10636 ) ;
#6907 = AXIS2_PLACEMENT_3D ( 'NONE', #1718, #6005, #1011 ) ;
#6908 = DIRECTION ( 'NONE',  ( 0.000000000000000000, 1.000000000000000000, -0.000000000000000000 ) ) ;
#6909 = CARTESIAN_POINT ( 'NONE',  ( 4.557748955467384455, 9.652551271539412170, -314.5171779026347281 ) ) ;
#6910 = ORIENTED_EDGE ( 'NONE', *, *, #5553, .F. ) ;
#6911 = CARTESIAN_POINT ( 'NONE',  ( 18.99998114578000141, -0.3144692935366000253, 190.0000000000100044 ) ) ;
#6912 = DIRECTION ( 'NONE',  ( 0.000000000000000000, 1.000000000000000000, 0.000000000000000000 ) ) ;
#6913 = EDGE_LOOP ( 'NONE', ( #1121, #1390 ) ) ;
#6914 = CARTESIAN_POINT ( 'NONE',  ( 13.99304003883001180, -8.933243331610997373, 191.1197171614399792 ) ) ;
#6915 = VERTEX_POINT ( 'NONE', #5405 ) ;
#6916 = CARTESIAN_POINT ( 'NONE',  ( -16.99953299605537183, -0.4334412736564766666, 315.0000000000000568 ) ) ;
#6917 = CARTESIAN_POINT ( 'NONE',  ( -14.28705177277001148, -7.417718350405998251, -302.5071922382879279 ) ) ;
#6918 = DIRECTION ( 'NONE',  ( -0.2951854283188049544, 0.000000000000000000, 0.9554399839384174475 ) ) ;
#6919 = VECTOR ( 'NONE', #8470, 1000.000000000000000 ) ;
#6920 = ADVANCED_FACE ( 'NONE', ( #8388 ), #4311, .T. ) ;
#6921 = CARTESIAN_POINT ( 'NONE',  ( -0.7165654159986467597, -7.501783096816999397, -434.1553209429059166 ) ) ;
#6922 = SURFACE_STYLE_FILL_AREA ( #6871 ) ;
#6923 = CARTESIAN_POINT ( 'NONE',  ( -45.40077937890500692, -9.000000000000001776, -426.7517346751886862 ) ) ;
#6924 = CARTESIAN_POINT ( 'NONE',  ( -19.97284365803998796, 0.5561741493802002667, 318.8802828394900644 ) ) ;
#6925 = CARTESIAN_POINT ( 'NONE',  ( 17.56758064089999749, -0.6313722887073999201, -314.4150829855000211 ) ) ;
#6926 = CARTESIAN_POINT ( 'NONE',  ( -15.27200851150000105, 4.387263554753999983, 314.8616023057000461 ) ) ;
#6927 = ORIENTED_EDGE ( 'NONE', *, *, #9496, .T. ) ;
#6928 = CARTESIAN_POINT ( 'NONE',  ( 4.683335428805002643, -11.03437642965999288, 190.0071920248299477 ) ) ;
#6929 = CARTESIAN_POINT ( 'NONE',  ( -0.7115441411924354753, -7.495838068657331377, -434.2340922344590695 ) ) ;
#6930 = EDGE_CURVE ( 'NONE', #2607, #6716, #230, .T. ) ;
#6931 = EDGE_CURVE ( 'NONE', #8108, #10456, #9264, .T. ) ;
#6932 = DIRECTION ( 'NONE',  ( 0.2381566831044910626, 0.000000000000000000, -0.9712267471052612455 ) ) ;
#6933 = CARTESIAN_POINT ( 'NONE',  ( -14.65007096172560708, 4.807726778454477490, 314.9999999999998863 ) ) ;
#6934 = CARTESIAN_POINT ( 'NONE',  ( 0.000000000000000000, 10.00000000000000000, 315.0000000000000000 ) ) ;
#6935 = CARTESIAN_POINT ( 'NONE',  ( -12.75178873474799168, -6.273979344207467612, -314.9999999999999432 ) ) ;
#6936 = DIRECTION ( 'NONE',  ( 0.8820010751365678914, 0.000000000000000000, 0.4712473909295818442 ) ) ;
#6937 = CARTESIAN_POINT ( 'NONE',  ( -73.93978370014021095, -12.50000000000000000, -368.3728591389038911 ) ) ;
#6938 = STYLED_ITEM ( 'NONE', ( #7247 ), #8498 ) ;
#6939 = LINE ( 'NONE', #8748, #5181 ) ;
#6940 = EDGE_CURVE ( 'NONE', #661, #2675, #3779, .T. ) ;
#6941 = CARTESIAN_POINT ( 'NONE',  ( -11.76997148278789673, 6.834709328092291258, -315.0000000000000000 ) ) ;
#6942 = CARTESIAN_POINT ( 'NONE',  ( -4.683335428805002643, 11.03437642965999288, 190.0071920248299477 ) ) ;
#6943 = FACE_OUTER_BOUND ( 'NONE', #4471, .T. ) ;
#6944 = AXIS2_PLACEMENT_3D ( 'NONE', #1091, #10073, #1958 ) ;
#6945 = ADVANCED_FACE ( 'NONE', ( #1327 ), #4608, .F. ) ;
#6946 = VECTOR ( 'NONE', #6956, 1000.000000000000114 ) ;
#6947 = MECHANICAL_DESIGN_GEOMETRIC_PRESENTATION_REPRESENTATION (  '', ( #8299 ), #9675 ) ;
#6948 = DIRECTION ( 'NONE',  ( 0.000000000000000000, -1.000000000000000000, 0.000000000000000000 ) ) ;
#6949 = AXIS2_PLACEMENT_3D ( 'NONE', #7783, #801, #2307 ) ;
#6950 = PLANE ( 'NONE',  #2628 ) ;
#6951 = CARTESIAN_POINT ( 'NONE',  ( 4.298491262593391760, -9.188587546143761386, 314.9999999999999432 ) ) ;
#6952 = CARTESIAN_POINT ( 'NONE',  ( -14.72449281369000040, 5.549439731021000632, -314.4150829855000211 ) ) ;
#6953 = EDGE_CURVE ( 'NONE', #8053, #8216, #9031, .T. ) ;
#6954 = ORIENTED_EDGE ( 'NONE', *, *, #2933, .T. ) ;
#6955 = CARTESIAN_POINT ( 'NONE',  ( -14.12295497348999440, 7.525186449763000773, 319.9928079742500131 ) ) ;
#6956 = DIRECTION ( 'NONE',  ( 0.2381566830310488381, -5.671339926113999656E-10, -0.9712267471232701732 ) ) ;
#6957 = CARTESIAN_POINT ( 'NONE',  ( -82.14476046060677561, -7.500000000000000000, -345.9384288226025888 ) ) ;
#6958 = VERTEX_POINT ( 'NONE', #4930 ) ;
#6959 = AXIS2_PLACEMENT_3D ( 'NONE', #8201, #839, #6591 ) ;
#6960 = CIRCLE ( 'NONE', #940, 3.500000000000003109 ) ;
#6961 = CARTESIAN_POINT ( 'NONE',  ( -17.77555462084998794, -5.884850558328997394, -317.0792622552969533 ) ) ;
#6962 = FACE_BOUND ( 'NONE', #110, .T. ) ;
#6963 = CARTESIAN_POINT ( 'NONE',  ( 13.47608353327720643, 6.291341891605557457, -314.5797986957608714 ) ) ;
#6964 = ORIENTED_EDGE ( 'NONE', *, *, #2731, .T. ) ;
#6965 = CARTESIAN_POINT ( 'NONE',  ( 7.592156631695000435, -10.54118908926000131, 190.0000000000000000 ) ) ;
#6966 = CARTESIAN_POINT ( 'NONE',  ( -19.14895805910627757, -3.641352296147344791, 319.0000000000003979 ) ) ;
#6967 = EDGE_CURVE ( 'NONE', #10131, #10253, #2740, .T. ) ;
#6968 = EDGE_LOOP ( 'NONE', ( #8500, #9497 ) ) ;
#6969 = CARTESIAN_POINT ( 'NONE',  ( 11.16929996816999804, -10.37059603288001419, 191.1197171614399792 ) ) ;
#6970 = ORIENTED_EDGE ( 'NONE', *, *, #5706, .F. ) ;
#6971 = CARTESIAN_POINT ( 'NONE',  ( 1.499999999999999556, -2.500000000000000000, -409.5000000000000568 ) ) ;
#6972 = CARTESIAN_POINT ( 'NONE',  ( -16.06615879071999231, -5.957812395457000143, -302.5071922382879279 ) ) ;
#6973 = CARTESIAN_POINT ( 'NONE',  ( -75.99363846394659561, -2.500000000000000000, -373.3662649509979587 ) ) ;
#6974 = B_SPLINE_CURVE_WITH_KNOTS ( 'NONE', 3,
 ( #4093, #9037, #4847, #2378, #2429, #8985, #759, #3233, #8177, #10538, #7070, #1309, #8122, #7371, #4148, #4043, #10337, #3283, #6509, #7320 ),
 .UNSPECIFIED., .F., .F.,
 ( 4, 1, 1, 1, 1, 1, 1, 2, 2, 1, 1, 2, 2, 4 ),
 ( 0.000000000000000000, 0.1250000000000086875, 0.1875000000000131006, 0.2187500000000181799, 0.2343750000000180134, 0.2421875000000205114, 0.2460937500000218159, 0.2480468750000249800, 0.2500000000000281442, 0.3750000000000131561, 0.4375000000000058287, 0.4687500000000042744, 0.5000000000000027756, 1.000000000000000000 ),
 .UNSPECIFIED. ) ;
#6975 = AXIS2_PLACEMENT_3D ( 'NONE', #605, #3066, #2262 ) ;
#6976 = DIRECTION ( 'NONE',  ( 0.000000000000000000, -1.000000000000000000, 0.000000000000000000 ) ) ;
#6977 =( BOUNDED_CURVE ( )  B_SPLINE_CURVE ( 3, ( #6860, #6145, #9432, #8668 ),
 .UNSPECIFIED., .F., .T. ) 
 B_SPLINE_CURVE_WITH_KNOTS ( ( 4, 4 ),
 ( 0.000000000000000000, 1.000000000000000000 ),
 .UNSPECIFIED. ) 
 CURVE ( )  GEOMETRIC_REPRESENTATION_ITEM ( )  RATIONAL_B_SPLINE_CURVE ( ( 1.000000000000000000, 0.8029010325775971513, 0.8003084355045908538, 0.9922222087809807745 ) ) 
 REPRESENTATION_ITEM ( '' )  );
#6978 = CARTESIAN_POINT ( 'NONE',  ( -17.62731894649998665, 4.091366980619998373, -302.5071922382879279 ) ) ;
#6979 = CARTESIAN_POINT ( 'NONE',  ( 9.940815099545000422, -10.93780185275999983, 319.5792614743400009 ) ) ;
#6980 = CARTESIAN_POINT ( 'NONE',  ( 16.80445917461999983, -3.015803745947999825, -314.4150829855000211 ) ) ;
#6981 = CARTESIAN_POINT ( 'NONE',  ( -3.971626792229000280, 9.186906450543000702, 315.0848619657999734 ) ) ;
#6982 = ORIENTED_EDGE ( 'NONE', *, *, #7327, .T. ) ;
#6983 = CARTESIAN_POINT ( 'NONE',  ( 13.41272981818000432, -7.983430642947998201, 190.0071920248299477 ) ) ;
#6984 = CARTESIAN_POINT ( 'NONE',  ( -16.30476707551000359, 7.243228625700997902, 318.8802828394900644 ) ) ;
#6985 = CARTESIAN_POINT ( 'NONE',  ( -13.30825372127758399, -9.000000000000001776, -400.6612558711213410 ) ) ;
#6986 = EDGE_CURVE ( 'NONE', #10485, #1864, #6376, .T. ) ;
#6987 = DIRECTION ( 'NONE',  ( 0.000000000000000000, 1.000000000000000000, -0.000000000000000000 ) ) ;
#6988 = CARTESIAN_POINT ( 'NONE',  ( -46.74071243419621169, -9.000000000000001776, -414.3237589990241077 ) ) ;
#6989 = CARTESIAN_POINT ( 'NONE',  ( -0.6597201369859407860, -2.500000714168999938, -434.1397697187372273 ) ) ;
#6990 = CARTESIAN_POINT ( 'NONE',  ( -11.69624556101560664, -6.874206995516637164, -315.0000000000000000 ) ) ;
#6991 = CARTESIAN_POINT ( 'NONE',  ( 20.00000000000000000, 0.000000000000000000, 319.0000000000000000 ) ) ;
#6992 = CARTESIAN_POINT ( 'NONE',  ( -20.40121062015000319, -2.500000000000000000, -430.0210166885000262 ) ) ;
#6993 = CARTESIAN_POINT ( 'NONE',  ( -3.713614856666575144E-09, 12.50000000000000000, -303.5000000000000000 ) ) ;
#6994 = CARTESIAN_POINT ( 'NONE',  ( -8.778856717165009371, 8.123403389731517876, -315.0000000000001137 ) ) ;
#6995 = PRODUCT_DEFINITION_SHAPE ( 'NONE', 'NONE',  #10635 ) ;
#6996 = CARTESIAN_POINT ( 'NONE',  ( -3.019104878445999063, 11.24894423506000152, 190.0071920248299477 ) ) ;
#6997 = CARTESIAN_POINT ( 'NONE',  ( 1.399293614871181202, -7.500000000000000000, -408.6664516090914390 ) ) ;
#6998 = ORIENTED_EDGE ( 'NONE', *, *, #4953, .F. ) ;
#6999 = CARTESIAN_POINT ( 'NONE',  ( -46.74071243419621169, -9.000000000000001776, -414.3237589990241077 ) ) ;
#7000 = EDGE_CURVE ( 'NONE', #8559, #10046, #7895, .T. ) ;
#7001 = DIRECTION ( 'NONE',  ( 0.9712267471052594692, 0.000000000000000000, 0.2381566831044984456 ) ) ;
#7002 = FILL_AREA_STYLE_COLOUR ( '', #5937 ) ;
#7003 = CARTESIAN_POINT ( 'NONE',  ( 3.309867371927075919, -9.320876041153052682, 315.0000000000000568 ) ) ;
#7004 = CARTESIAN_POINT ( 'NONE',  ( -12.28828818102000042, 7.249309191407999897, -314.4150829855000211 ) ) ;
#7005 = CIRCLE ( 'NONE', #2882, 0.5000000000000066613 ) ;
#7006 = DIRECTION ( 'NONE',  ( 0.000000000000000000, 0.000000000000000000, -1.000000000000000000 ) ) ;
#7007 = DIRECTION ( 'NONE',  ( 1.000000000000000000, 0.000000000000000000, 0.000000000000000000 ) ) ;
#7008 = DIRECTION ( 'NONE',  ( -0.000000000000000000, 1.000000000000000000, -0.000000000000000000 ) ) ;
#7009 = EDGE_LOOP ( 'NONE', ( #9858, #7310, #620, #5712 ) ) ;
#7010 = CARTESIAN_POINT ( 'NONE',  ( -14.32792941690000177, 7.389020440446000926, -317.4928077629770087 ) ) ;
#7011 = CARTESIAN_POINT ( 'NONE',  ( -3.365463313584999838, -12.41489380075000604, -317.0792622552969533 ) ) ;
#7012 = ADVANCED_FACE ( 'NONE', ( #1496 ), #2358, .T. ) ;
#7013 = DIRECTION ( 'NONE',  ( -0.7784864941890657919, 0.000000000000000000, -0.6276613564377032661 ) ) ;
#7014 = EDGE_CURVE ( 'NONE', #6311, #6305, #9894, .T. ) ;
#7015 = CARTESIAN_POINT ( 'NONE',  ( -10.00000000000000000, 2.500000000000000000, -317.5000000000000000 ) ) ;
#7016 = VERTEX_POINT ( 'NONE', #6544 ) ;
#7017 = CARTESIAN_POINT ( 'NONE',  ( -17.81342281586000098, -3.988456401492999959, 190.0000000000000000 ) ) ;
#7018 = LINE ( 'NONE', #5333, #2140 ) ;
#7019 = ORIENTED_EDGE ( 'NONE', *, *, #1577, .F. ) ;
#7020 = CARTESIAN_POINT ( 'NONE',  ( -17.64332610462000872, -5.892819363352002959, 191.1197171614399792 ) ) ;
#7021 = EDGE_LOOP ( 'NONE', ( #9713, #633, #6480, #3493 ) ) ;
#7022 = CARTESIAN_POINT ( 'NONE',  ( -17.50000000088854435, -5.867334121986941042, -302.5000000000002842 ) ) ;
#7023 = CARTESIAN_POINT ( 'NONE',  ( -15.21156667173000621, -6.719223644262998008, -302.5071922382879279 ) ) ;
#7024 = CARTESIAN_POINT ( 'NONE',  ( 28.53863984632670636, -2.500000000000000000, -506.8274460463252353 ) ) ;
#7025 = ADVANCED_FACE ( 'NONE', ( #4774 ), #6318, .F. ) ;
#7026 = DIRECTION ( 'NONE',  ( 0.000000000000000000, 1.000000000000000000, -0.000000000000000000 ) ) ;
#7027 =( NAMED_UNIT ( * ) SI_UNIT ( $, .STERADIAN. ) SOLID_ANGLE_UNIT ( ) );
#7028 = CARTESIAN_POINT ( 'NONE',  ( -15.25170542629001602, 6.686182281419003282, -302.5071922382879279 ) ) ;
#7029 = CARTESIAN_POINT ( 'NONE',  ( -15.65693014362998348, -7.780815921226000853, 318.8802828394900644 ) ) ;
#7030 = CARTESIAN_POINT ( 'NONE',  ( 15.60185585328000002, -4.689707898928999974, -314.4150829855000211 ) ) ;
#7031 = CARTESIAN_POINT ( 'NONE',  ( -16.77957632114000219, 1.244976636274000015, 315.0848619657999734 ) ) ;
#7032 = ORIENTED_EDGE ( 'NONE', *, *, #3893, .F. ) ;
#7033 = CARTESIAN_POINT ( 'NONE',  ( 3.019104878445999063, -11.24894423506000152, 190.0071920248299477 ) ) ;
#7034 = ORIENTED_EDGE ( 'NONE', *, *, #2464, .F. ) ;
#7035 = CARTESIAN_POINT ( 'NONE',  ( -0.9751833592927913186, -7.478962837042861800, -434.3989537440571667 ) ) ;
#7036 = DIRECTION ( 'NONE',  ( 0.000000000000000000, -1.000000000000000000, 0.000000000000000000 ) ) ;
#7037 = CIRCLE ( 'NONE', #5648, 4.000000000000000000 ) ;
#7038 = CARTESIAN_POINT ( 'NONE',  ( -16.90189876424999937, 0.3838616842170000099, 315.0848619657999734 ) ) ;
#7039 = CARTESIAN_POINT ( 'NONE',  ( -75.99363846394659561, -7.500000000000000000, -373.3662649509979587 ) ) ;
#7040 = CYLINDRICAL_SURFACE ( 'NONE', #2958, 3.500000000000003109 ) ;
#7041 = DIRECTION ( 'NONE',  ( 0.000000000000000000, -1.000000000000000000, 0.000000000000000000 ) ) ;
#7042 = AXIS2_PLACEMENT_3D ( 'NONE', #4025, #4832, #6496 ) ;
#7043 = CARTESIAN_POINT ( 'NONE',  ( -11.54764063961475351, -6.952680983979390383, -315.0000000000000000 ) ) ;
#7044 = CARTESIAN_POINT ( 'NONE',  ( -5.178550450922173809, -3.174732006113173188, -436.6812520500867549 ) ) ;
#7045 = CARTESIAN_POINT ( 'NONE',  ( 17.16661504264608951, -5.088157148453773714E-08, 314.8332817084516364 ) ) ;
#7046 = CARTESIAN_POINT ( 'NONE',  ( -3.784291777249242816, -6.824938403275000454, -436.5423981522574763 ) ) ;
#7047 = CARTESIAN_POINT ( 'NONE',  ( 6.369817261971415512, 8.818538635844451079, -315.0000000000000000 ) ) ;
#7048 = CARTESIAN_POINT ( 'NONE',  ( 12.81613682183999536, 9.130924732858002102, 189.9229057364800042 ) ) ;
#7049 = DIRECTION ( 'NONE',  ( 0.000000000000000000, 1.000000000000000000, 0.000000000000000000 ) ) ;
#7050 = CIRCLE ( 'NONE', #8753, 3.500000000000003109 ) ;
#7051 = ORIENTED_EDGE ( 'NONE', *, *, #4315, .F. ) ;
#7052 = LINE ( 'NONE', #2049, #5271 ) ;
#7053 = AXIS2_PLACEMENT_3D ( 'NONE', #5803, #6564, #65 ) ;
#7054 = EDGE_CURVE ( 'NONE', #9639, #1033, #8728, .T. ) ;
#7055 = CARTESIAN_POINT ( 'NONE',  ( -45.24937426871918689, -7.500000000000000000, -448.9804009737068213 ) ) ;
#7056 = SURFACE_STYLE_FILL_AREA ( #8651 ) ;
#7057 = CARTESIAN_POINT ( 'NONE',  ( 8.096811247556559010, -8.344189070382460827, 315.0000000000001137 ) ) ;
#7058 = CARTESIAN_POINT ( 'NONE',  ( -6.438474686349000997, 8.964777275824999947, -314.8616023057000461 ) ) ;
#7059 = CARTESIAN_POINT ( 'NONE',  ( -19.08872200864999868, -2.500000000000000000, -429.3350920981999934 ) ) ;
#7060 = CARTESIAN_POINT ( 'NONE',  ( 16.74680747859001784, 6.256295688540001620, 320.0770942683900557 ) ) ;
#7061 = LINE ( 'NONE', #10278, #74 ) ;
#7062 = CARTESIAN_POINT ( 'NONE',  ( -1.050554280480674452, -2.604844966689999097, -434.8275985566710347 ) ) ;
#7063 = EDGE_LOOP ( 'NONE', ( #6998, #5762, #6087, #8084 ) ) ;
#7064 = CARTESIAN_POINT ( 'NONE',  ( 3.312898553962003056, 11.91959439673999199, -317.5770954168139610 ) ) ;
#7065 = CARTESIAN_POINT ( 'NONE',  ( -16.55682536756000545, -6.456981081556999236, -317.5770954168139610 ) ) ;
#7066 = EDGE_CURVE ( 'NONE', #8626, #306, #529, .T. ) ;
#7067 = PLANE ( 'NONE',  #8697 ) ;
#7068 = CARTESIAN_POINT ( 'NONE',  ( 6.052780067456072999, -5.500000000000000000, -524.2189112390747141 ) ) ;
#7069 = VERTEX_POINT ( 'NONE', #844 ) ;
#7070 = CARTESIAN_POINT ( 'NONE',  ( -3.753597148019404806, -7.027035274121325337, -436.1383244323657777 ) ) ;
#7071 = CARTESIAN_POINT ( 'NONE',  ( 6.040317665795909008, -11.93081507280030884, 319.0000000000003979 ) ) ;
#7072 = ORIENTED_EDGE ( 'NONE', *, *, #5368, .T. ) ;
#7073 = CARTESIAN_POINT ( 'NONE',  ( -19.98293839508998104, 0.4162045188174002819, 191.1197171614399792 ) ) ;
#7074 = ORIENTED_EDGE ( 'NONE', *, *, #5368, .F. ) ;
#7075 = CARTESIAN_POINT ( 'NONE',  ( -16.99996037728000076, 1.352916227065999958E-09, 314.9999801883000146 ) ) ;
#7076 = CARTESIAN_POINT ( 'NONE',  ( -14.68756396110000395, -7.991310926523999214, -302.4229045757450081 ) ) ;
#7077 = EDGE_CURVE ( 'NONE', #5864, #10381, #1379, .T. ) ;
#7078 = DIRECTION ( 'NONE',  ( 0.4716280258120412183, 0.000000000000000000, -0.8817975988108815999 ) ) ;
#7079 = VECTOR ( 'NONE', #10471, 1000.000000000000000 ) ;
#7080 = ORIENTED_EDGE ( 'NONE', *, *, #977, .F. ) ;
#7081 = CARTESIAN_POINT ( 'NONE',  ( -0.8648435279641549789, -7.423678894978000820, -434.7417815575237796 ) ) ;
#7082 = CARTESIAN_POINT ( 'NONE',  ( 18.91993355959997558, 3.215835268190998075, -302.4229045757450081 ) ) ;
#7083 = PRODUCT_DEFINITION_SHAPE ( 'NONE', 'NONE',  #10626 ) ;
#7084 = CARTESIAN_POINT ( 'NONE',  ( -76.74404526914973701, -8.000000000000000000, -359.2961792914830426 ) ) ;
#7085 = VECTOR ( 'NONE', #1640, 1000.000000000000000 ) ;
#7086 = CARTESIAN_POINT ( 'NONE',  ( -8.450675645183000739, -8.177559542660000957, -315.0848619657999734 ) ) ;
#7087 = CARTESIAN_POINT ( 'NONE',  ( -12.07130791617000121, 6.858215270785999351, 314.8616023057000461 ) ) ;
#7088 = AXIS2_PLACEMENT_3D ( 'NONE', #4514, #7794, #7001 ) ;
#7089 = ORIENTED_EDGE ( 'NONE', *, *, #7629, .T. ) ;
#7090 = CARTESIAN_POINT ( 'NONE',  ( 17.27977314787002427, -4.562413721234999109, 190.0071920248299477 ) ) ;
#7091 = CARTESIAN_POINT ( 'NONE',  ( -0.6578543451058023184, -7.499974772742706186, -434.1490756834378431 ) ) ;
#7092 = FACE_OUTER_BOUND ( 'NONE', #2401, .T. ) ;
#7093 = VECTOR ( 'NONE', #6001, 1000.000000000000000 ) ;
#7094 = CYLINDRICAL_SURFACE ( 'NONE', #4598, 3.500000000000006217 ) ;
#7095 = DIRECTION ( 'NONE',  ( -1.000000000000000000, 0.000000000000000000, 0.000000000000000000 ) ) ;
#7096 = CARTESIAN_POINT ( 'NONE',  ( 13.57573464316000056, -3.225916527208000151, 315.0000000000001705 ) ) ;
#7097 = CARTESIAN_POINT ( 'NONE',  ( -15.06645494800451068, -4.378519400638149150, -315.0000000000000568 ) ) ;
#7098 = DIRECTION ( 'NONE',  ( 0.000000000000000000, -1.000000000000000000, 0.000000000000000000 ) ) ;
#7099 = CARTESIAN_POINT ( 'NONE',  ( -12.95168232056959212, -5.749022766740000456, -439.0697820409906171 ) ) ;
#7100 = CARTESIAN_POINT ( 'NONE',  ( -11.78094678683302376, 6.828785851005065410, -315.0000000000000000 ) ) ;
#7101 = CARTESIAN_POINT ( 'NONE',  ( -16.71231899867997583, 6.291214601299001785, 189.9229057364800042 ) ) ;
#7102 = CARTESIAN_POINT ( 'NONE',  ( 5.453091995311539542, 9.512452488116691640, 314.4999455543127738 ) ) ;
#7103 = CARTESIAN_POINT ( 'NONE',  ( 6.537962633339999385, -10.80030782989000038, -317.5000000000000000 ) ) ;
#7104 = DIRECTION ( 'NONE',  ( 0.000000000000000000, 1.000000000000000000, -0.000000000000000000 ) ) ;
#7105 =( GEOMETRIC_REPRESENTATION_CONTEXT ( 3 ) GLOBAL_UNCERTAINTY_ASSIGNED_CONTEXT ( ( #4317 ) ) GLOBAL_UNIT_ASSIGNED_CONTEXT ( ( #1657, #2412, #1609 ) ) REPRESENTATION_CONTEXT ( 'NONE', 'WORKASPACE' ) );
#7106 = CARTESIAN_POINT ( 'NONE',  ( 15.35630118782766651, -4.050343336346089451, 315.0000000000000000 ) ) ;
#7107 = CARTESIAN_POINT ( 'NONE',  ( 11.89238025184999792, 6.701939844102000166, -315.0848619657999734 ) ) ;
#7108 = FACE_OUTER_BOUND ( 'NONE', #10386, .T. ) ;
#7109 = CARTESIAN_POINT ( 'NONE',  ( -17.84276444133998041, 4.978015457891998174, 320.0770942683900557 ) ) ;
#7110 = CARTESIAN_POINT ( 'NONE',  ( -14.85829447703713235, -5.615530704401715312, -438.9414600939686011 ) ) ;
#7111 = VECTOR ( 'NONE', #6744, 1000.000000000000227 ) ;
#7112 = CARTESIAN_POINT ( 'NONE',  ( -0.6495235857412369196, -2.539793227551998545, -434.6255535651486639 ) ) ;
#7113 = VERTEX_POINT ( 'NONE', #9019 ) ;
#7114 = CARTESIAN_POINT ( 'NONE',  ( -15.69339834701000136, 7.228928788388996551, -317.5770954168139610 ) ) ;
#7115 = CARTESIAN_POINT ( 'NONE',  ( -10.46141074968000062, -10.65879569097000079, -316.3802825947000201 ) ) ;
#7116 = AXIS2_PLACEMENT_3D ( 'NONE', #1569, #711, #3983 ) ;
#7117 = CARTESIAN_POINT ( 'NONE',  ( 19.99999035944999903, -7.277437094418000096E-10, -303.5000000000000000 ) ) ;
#7118 = CARTESIAN_POINT ( 'NONE',  ( -41.12300563599592351, -9.500000000000001776, -403.1572299801428017 ) ) ;
#7119 = VECTOR ( 'NONE', #352, 1000.000000000000000 ) ;
#7120 = ORIENTED_EDGE ( 'NONE', *, *, #342, .F. ) ;
#7121 = CARTESIAN_POINT ( 'NONE',  ( -10.00000000000000000, 2.500000000000000000, -317.5000000000000000 ) ) ;
#7122 = DIRECTION ( 'NONE',  ( 0.000000000000000000, -1.000000000000000000, 0.000000000000000000 ) ) ;
#7123 = EDGE_LOOP ( 'NONE', ( #10605, #4403, #5799, #4282 ) ) ;
#7124 = CARTESIAN_POINT ( 'NONE',  ( -19.00000000000000000, 0.000000000000000000, -317.4999999998989892 ) ) ;
#7125 = ORIENTED_EDGE ( 'NONE', *, *, #6623, .F. ) ;
#7126 = CARTESIAN_POINT ( 'NONE',  ( -11.77008734995756178, -6.834641529527616832, 315.0000000000000568 ) ) ;
#7127 = CARTESIAN_POINT ( 'NONE',  ( 19.60208457603997090, -0.3236162399036999759, -302.4229045757450081 ) ) ;
#7128 = CARTESIAN_POINT ( 'NONE',  ( 9.971838575284008854, 10.83713921150001447, 191.1197171614399792 ) ) ;
#7129 = EDGE_CURVE ( 'NONE', #10404, #9387, #360, .T. ) ;
#7130 = CARTESIAN_POINT ( 'NONE',  ( -14.73495828939998731, 7.957952820716998055, -302.4229045757450081 ) ) ;
#7131 = CARTESIAN_POINT ( 'NONE',  ( 0.6337574957234999307, -12.50712592802002021, 318.8802828394900644 ) ) ;
#7132 = ORIENTED_EDGE ( 'NONE', *, *, #10035, .F. ) ;
#7133 = CARTESIAN_POINT ( 'NONE',  ( -14.52969073417999901, -5.422537850045999974, -314.6383426456000052 ) ) ;
#7134 = LINE ( 'NONE', #9654, #5386 ) ;
#7135 = EDGE_CURVE ( 'NONE', #8191, #1416, #2757, .T. ) ;
#7136 = ORIENTED_EDGE ( 'NONE', *, *, #5162, .F. ) ;
#7137 = CARTESIAN_POINT ( 'NONE',  ( -19.11670425725001010, -2.646693943201001264, 189.9229057364800042 ) ) ;
#7138 = CARTESIAN_POINT ( 'NONE',  ( -11.17208682466014302, 10.37722895585535809, 190.9999999999996589 ) ) ;
#7139 = CARTESIAN_POINT ( 'NONE',  ( 10.00000000000000000, -2.500000000000000000, -285.0000000000000000 ) ) ;
#7140 = ADVANCED_FACE ( 'NONE', ( #5513 ), #9659, .F. ) ;
#7141 = CARTESIAN_POINT ( 'NONE',  ( -16.07469914181999826, -3.754035329064000059, 314.6383426456000052 ) ) ;
#7142 = DIRECTION ( 'NONE',  ( 0.000000000000000000, 0.000000000000000000, -1.000000000000000000 ) ) ;
#7143 = CARTESIAN_POINT ( 'NONE',  ( -16.47320456655591059, 2.338720490045835820, 314.9999999999999432 ) ) ;
#7144 = CARTESIAN_POINT ( 'NONE',  ( -17.42228208267999889, -1.444224815522999972, 314.4150829855000211 ) ) ;
#7145 = CARTESIAN_POINT ( 'NONE',  ( -16.13978190921855216, -2.966266463780214302, -315.0000000000000000 ) ) ;
#7146 = CARTESIAN_POINT ( 'NONE',  ( -14.88932286584991438, -4.303667523461871980, -438.8149232244517179 ) ) ;
#7147 = CYLINDRICAL_SURFACE ( 'NONE', #420, 3.499999999999999112 ) ;
#7148 = EDGE_LOOP ( 'NONE', ( #560, #9484, #1563, #5092 ) ) ;
#7149 = CARTESIAN_POINT ( 'NONE',  ( -100.2082379103963063, -2.500000000000000000, -339.7166298527751565 ) ) ;
#7150 = CARTESIAN_POINT ( 'NONE',  ( -8.717693564518029348, 8.144027366771089405, -314.9999999999999432 ) ) ;
#7151 = CARTESIAN_POINT ( 'NONE',  ( -18.24410766404003326, 5.273389473771006308, 190.4207385301700128 ) ) ;
#7152 = CARTESIAN_POINT ( 'NONE',  ( 8.203499347305186262, 8.842483610386494775, 314.4999460608030404 ) ) ;
#7153 = CARTESIAN_POINT ( 'NONE',  ( -11.71572875140193837, -12.50000000114647847, -316.5000000000000000 ) ) ;
#7154 = DIRECTION ( 'NONE',  ( 0.4712473909295827323, 0.000000000000000000, -0.8820010751365675583 ) ) ;
#7155 = EDGE_CURVE ( 'NONE', #10171, #7605, #2222, .T. ) ;
#7156 = CARTESIAN_POINT ( 'NONE',  ( 316.6938378867111510, 4.999999999999993783, -318.8136152473334164 ) ) ;
#7157 = CARTESIAN_POINT ( 'NONE',  ( 16.95904175860000151, 2.156867278632000229, -314.6383426456000052 ) ) ;
#7158 = FACE_OUTER_BOUND ( 'NONE', #9944, .T. ) ;
#7159 = CARTESIAN_POINT ( 'NONE',  ( -8.650961417647998530, 10.84061383582999838, 320.0770942683900557 ) ) ;
#7160 = CARTESIAN_POINT ( 'NONE',  ( -14.76420639513456301, -5.500000000000000000, -439.3251606919798178 ) ) ;
#7161 = CARTESIAN_POINT ( 'NONE',  ( -1.111851599903384891, -2.511083096523998748, -434.4041198421772947 ) ) ;
#7162 = ORIENTED_EDGE ( 'NONE', *, *, #5420, .T. ) ;
#7163 = CARTESIAN_POINT ( 'NONE',  ( -12.67153153313999070, 9.210367834107003659, -317.5770954168139610 ) ) ;
#7164 = CARTESIAN_POINT ( 'NONE',  ( -3.356563794682998925, -12.33103673683000423, -316.3802825947000201 ) ) ;
#7165 = PRODUCT_DEFINITION_SHAPE ( 'NONE', 'NONE',  #8684 ) ;
#7166 = EDGE_LOOP ( 'NONE', ( #7516, #1039, #9196, #4391 ) ) ;
#7167 = CYLINDRICAL_SURFACE ( 'NONE', #1678, 12.49999999999998579 ) ;
#7168 = AXIS2_PLACEMENT_3D ( 'NONE', #6676, #7692, #5003 ) ;
#7169 = CARTESIAN_POINT ( 'NONE',  ( -11.51453371961019556, 7.479120141997829485, -314.5676927934668470 ) ) ;
#7170 = EDGE_CURVE ( 'NONE', #3141, #8899, #9770, .T. ) ;
#7171 = EDGE_LOOP ( 'NONE', ( #4105, #5565, #4531, #8461 ) ) ;
#7172 = CARTESIAN_POINT ( 'NONE',  ( -64.74703706733102138, -8.000000000000000000, -381.8372235071499290 ) ) ;
#7173 = ORIENTED_EDGE ( 'NONE', *, *, #5332, .F. ) ;
#7174 = CARTESIAN_POINT ( 'NONE',  ( -6.752884998590674925, 11.77766676623698139, -316.5000000000004547 ) ) ;
#7175 = EDGE_LOOP ( 'NONE', ( #2066, #6351, #1836, #4476 ) ) ;
#7176 = CARTESIAN_POINT ( 'NONE',  ( -5.850395566949658566, -8.918560297860793185, 315.0000000000000000 ) ) ;
#7177 = CARTESIAN_POINT ( 'NONE',  ( -9.338997116452000924, -11.14661793222000519, -302.9207377450070453 ) ) ;
#7178 = LINE ( 'NONE', #8894, #5211 ) ;
#7179 = VECTOR ( 'NONE', #6976, 1000.000000000000000 ) ;
#7180 = VERTEX_POINT ( 'NONE', #9716 ) ;
#7181 = EDGE_CURVE ( 'NONE', #4512, #1396, #5676, .T. ) ;
#7182 = CARTESIAN_POINT ( 'NONE',  ( 6.596975511883001353, 11.38119116100000028, -302.4229045757450081 ) ) ;
#7183 = CARTESIAN_POINT ( 'NONE',  ( -7.846787046322997838, -11.50147725199999371, 318.8802828394900644 ) ) ;
#7184 = ORIENTED_EDGE ( 'NONE', *, *, #5688, .T. ) ;
#7185 = CARTESIAN_POINT ( 'NONE',  ( -3.874983216044999956, -9.425407904674999671, -314.8616023057000461 ) ) ;
#7186 = CARTESIAN_POINT ( 'NONE',  ( 16.89041368998000081, 5.257268626091000208, -302.5000000000009663 ) ) ;
#7187 = ORIENTED_EDGE ( 'NONE', *, *, #5943, .F. ) ;
#7188 = CARTESIAN_POINT ( 'NONE',  ( -11.86325706386000434, -9.609314883874001012, 189.9229057364800042 ) ) ;
#7189 = CARTESIAN_POINT ( 'NONE',  ( -9.013443235573840084, 11.16848941897283076, 190.9999999999996589 ) ) ;
#7190 = CARTESIAN_POINT ( 'NONE',  ( -28.01838671672000203, -2.500000000000000000, -497.7560445212000104 ) ) ;
#7191 = ADVANCED_FACE ( 'NONE', ( #4879 ), #8157, .T. ) ;
#7192 = EDGE_CURVE ( 'NONE', #111, #4424, #6706, .T. ) ;
#7193 = ORIENTED_EDGE ( 'NONE', *, *, #7851, .T. ) ;
#7194 = CARTESIAN_POINT ( 'NONE',  ( -10.58801790939999954, -8.088125079530000150, 314.4150829855000211 ) ) ;
#7195 = CARTESIAN_POINT ( 'NONE',  ( -18.78787853991000034, 1.761062637770999917, 320.0000000000000000 ) ) ;
#7196 = CARTESIAN_POINT ( 'NONE',  ( 4.237945188771000460, -11.10223611999999704, 319.9928079742500131 ) ) ;
#7197 = CARTESIAN_POINT ( 'NONE',  ( -17.61684826078804988, 5.934684944789588634, 319.0000000000005116 ) ) ;
#7198 = CARTESIAN_POINT ( 'NONE',  ( 10.23467949614886763, -10.00000000050611781, -302.4999999999996021 ) ) ;
#7199 = DIRECTION ( 'NONE',  ( 0.000000000000000000, 0.000000000000000000, -1.000000000000000000 ) ) ;
#7200 = ORIENTED_EDGE ( 'NONE', *, *, #9836, .T. ) ;
#7201 = DIRECTION ( 'NONE',  ( -0.000000000000000000, 1.000000000000000000, 0.000000000000000000 ) ) ;
#7202 = VECTOR ( 'NONE', #923, 1000.000000000000000 ) ;
#7203 = CIRCLE ( 'NONE', #4452, 3.500000000000020428 ) ;
#7204 = CARTESIAN_POINT ( 'NONE',  ( 15.34534221234999585, 7.499749350177997265, 189.9229057364800042 ) ) ;
#7205 = CARTESIAN_POINT ( 'NONE',  ( -17.33381025012258903, -7.500000000000000000, -445.8348527500487535 ) ) ;
#7206 = EDGE_CURVE ( 'NONE', #5548, #3094, #3375, .T. ) ;
#7207 = FACE_BOUND ( 'NONE', #5773, .T. ) ;
#7208 = VECTOR ( 'NONE', #7902, 1000.000000000000114 ) ;
#7209 = CARTESIAN_POINT ( 'NONE',  ( 15.60753896450557221, 3.741771784933492828, 315.0000000000000568 ) ) ;
#7210 = PRODUCT_CONTEXT ( 'NONE', #14, 'mechanical' ) ;
#7211 = DIRECTION ( 'NONE',  ( 0.000000000000000000, -1.000000000000000000, 0.000000000000000000 ) ) ;
#7212 = CARTESIAN_POINT ( 'NONE',  ( -19.00000000000000000, 0.000000000000000000, -302.5000000001010108 ) ) ;
#7213 = CARTESIAN_POINT ( 'NONE',  ( -41.41721991556968874, -12.00000000000000000, -366.3159076589344636 ) ) ;
#7214 = CARTESIAN_POINT ( 'NONE',  ( 1.310287062331999319, 12.07175205226999815, 320.0770942683900557 ) ) ;
#7215 = CARTESIAN_POINT ( 'NONE',  ( -72.90663470096859555, -7.500000000000000000, -371.7168990827444190 ) ) ;
#7216 = CARTESIAN_POINT ( 'NONE',  ( -0.3553996609399175943, -2.459433156087002192, -433.9334582789244905 ) ) ;
#7217 = EDGE_LOOP ( 'NONE', ( #448, #5621, #6212, #455 ) ) ;
#7218 = CARTESIAN_POINT ( 'NONE',  ( 6.380917221297004005, 11.42904134337998734, -317.5770954168139610 ) ) ;
#7219 = VECTOR ( 'NONE', #4896, 1000.000000000000114 ) ;
#7220 = CARTESIAN_POINT ( 'NONE',  ( -16.84537440012000786, -6.754000406595005224, -316.3802825947000201 ) ) ;
#7221 = ORIENTED_EDGE ( 'NONE', *, *, #4052, .F. ) ;
#7222 = CARTESIAN_POINT ( 'NONE',  ( 10.58225433500999912, -9.538747186136999900, 320.0000000000000000 ) ) ;
#7223 = PRODUCT_DEFINITION_CONTEXT ( 'detailed design', #4695, 'design' ) ;
#7224 = DIRECTION ( 'NONE',  ( 0.6276613564377028220, 0.000000000000000000, -0.7784864941890661250 ) ) ;
#7225 = CARTESIAN_POINT ( 'NONE',  ( -7.237892782308162687, 9.087442202657104673, -314.5335583295244533 ) ) ;
#7226 = ORIENTED_EDGE ( 'NONE', *, *, #1880, .T. ) ;
#7227 = CARTESIAN_POINT ( 'NONE',  ( 11.98824862436842409, -10.01561519341996132, 319.0000000000003979 ) ) ;
#7228 = EDGE_LOOP ( 'NONE', ( #4285, #6110, #3697, #907, #1253, #6879, #7162 ) ) ;
#7229 = CARTESIAN_POINT ( 'NONE',  ( -72.90663470102438737, -7.500000000000000888, -371.7168990826883714 ) ) ;
#7230 = EDGE_LOOP ( 'NONE', ( #7193, #3723, #8448, #4701, #6214, #5899 ) ) ;
#7231 = CARTESIAN_POINT ( 'NONE',  ( -11.84516230667378345, -6.793967159201454997, 315.0000000000000568 ) ) ;
#7232 = CARTESIAN_POINT ( 'NONE',  ( 3.382256884648001893, -11.91212135210998824, -302.4229045757450081 ) ) ;
#7233 = LINE ( 'NONE', #9810, #6592 ) ;
#7234 = CARTESIAN_POINT ( 'NONE',  ( 7.006889269069000115, -6.844138725329000472, 315.0000000000000000 ) ) ;
#7235 = CARTESIAN_POINT ( 'NONE',  ( -7.947966332010000023, 11.56278913298000077, -302.9207377450070453 ) ) ;
#7236 = CARTESIAN_POINT ( 'NONE',  ( 16.30476707551000359, -7.243228625700997902, 318.8802828394900644 ) ) ;
#7237 = ORIENTED_EDGE ( 'NONE', *, *, #1252, .T. ) ;
#7238 = CARTESIAN_POINT ( 'NONE',  ( 1.399029207469000058, -9.644928263550999858, -314.8616023057000461 ) ) ;
#7239 = DIRECTION ( 'NONE',  ( -0.5828070674935414974, 0.000000000000000000, -0.8126105599114366029 ) ) ;
#7240 = VERTEX_POINT ( 'NONE', #8257 ) ;
#7241 = CARTESIAN_POINT ( 'NONE',  ( -14.56080423438999993, -8.072998568875000558, 189.9229057364800042 ) ) ;
#7242 = CARTESIAN_POINT ( 'NONE',  ( -1.249193831065315452, 12.49557363514548491, 190.9999999999996589 ) ) ;
#7243 = DIRECTION ( 'NONE',  ( 0.000000000000000000, 1.000000000000000000, -0.000000000000000000 ) ) ;
#7244 = EDGE_CURVE ( 'NONE', #726, #5350, #7037, .T. ) ;
#7245 = AXIS2_PLACEMENT_3D ( 'NONE', #1505, #3225, #5686 ) ;
#7246 = CARTESIAN_POINT ( 'NONE',  ( -16.25556153634000367, -3.885850782616000032, 314.4150829855000211 ) ) ;
#7247 = PRESENTATION_STYLE_ASSIGNMENT (( #4778 ) ) ;
#7248 = CARTESIAN_POINT ( 'NONE',  ( 3.142739053800999827, 11.35686622240999810, 320.0000000000000000 ) ) ;
#7249 = CARTESIAN_POINT ( 'NONE',  ( 13.31009360926000085, -8.046300872832002682, 319.9928079742500131 ) ) ;
#7250 = ADVANCED_BREP_SHAPE_REPRESENTATION ( '', ( #8714, #2817 ), #8667 ) ;
#7251 = DIRECTION ( 'NONE',  ( -0.09270529807100655328, 0.000000000000000000, 0.9956935912767369556 ) ) ;
#7252 = CARTESIAN_POINT ( 'NONE',  ( -14.98500449093754838, -3.629407339799118226, -438.4247239981262965 ) ) ;
#7253 = DIRECTION ( 'NONE',  ( 0.000000000000000000, 1.000000000000000000, 0.000000000000000000 ) ) ;
#7254 = ORIENTED_EDGE ( 'NONE', *, *, #2346, .F. ) ;
#7255 = CARTESIAN_POINT ( 'NONE',  ( 7.006889269069000115, 6.844138725329000472, -285.0000000000000000 ) ) ;
#7256 = EDGE_CURVE ( 'NONE', #9641, #9136, #1760, .T. ) ;
#7257 = CARTESIAN_POINT ( 'NONE',  ( -11.00905209676000140, 9.989194338198000622, 189.9229057364800042 ) ) ;
#7258 = CYLINDRICAL_SURFACE ( 'NONE', #7456, 4.000000000000008882 ) ;
#7259 = CIRCLE ( 'NONE', #7427, 3.500000000000020428 ) ;
#7260 = CARTESIAN_POINT ( 'NONE',  ( -11.71572875140193837, -12.50000000114647847, -303.4999999999999432 ) ) ;
#7261 = CARTESIAN_POINT ( 'NONE',  ( 16.39045651208371979, 2.501479531468998818, 315.0000000000000000 ) ) ;
#7262 = APPLICATION_PROTOCOL_DEFINITION ( 'draft international standard', 'automotive_design', 1998, #6331 ) ;
#7263 = CARTESIAN_POINT ( 'NONE',  ( -19.30523607465251956, -3.390426274888738156, -303.5000000000006253 ) ) ;
#7264 = CARTESIAN_POINT ( 'NONE',  ( 16.25556153634000367, 3.885850782616000032, -314.4150829855000211 ) ) ;
#7265 = ADVANCED_FACE ( 'NONE', ( #950 ), #3599, .T. ) ;
#7266 = CARTESIAN_POINT ( 'NONE',  ( -10.81481884307000207, 10.07000335707000538, 320.0770942683900557 ) ) ;
#7267 = CARTESIAN_POINT ( 'NONE',  ( 10.00000000000000000, 2.500000000000000000, -285.0000000000000000 ) ) ;
#7268 = ADVANCED_FACE ( 'NONE', ( #3318 ), #895, .T. ) ;
#7269 = CARTESIAN_POINT ( 'NONE',  ( -0.4853341206058132129, -2.507971610063000956, -434.5088091749634600 ) ) ;
#7270 = ORIENTED_EDGE ( 'NONE', *, *, #6694, .T. ) ;
#7271 = CARTESIAN_POINT ( 'NONE',  ( 11.66516470684000772, 10.15894662545001381, -316.3802825947000201 ) ) ;
#7272 = CARTESIAN_POINT ( 'NONE',  ( -19.86719273998999213, -1.743644188460999667, -316.3802825947000201 ) ) ;
#7273 = AXIS2_PLACEMENT_3D ( 'NONE', #1439, #7832, #7142 ) ;
#7274 = CARTESIAN_POINT ( 'NONE',  ( -15.00000000000000000, 0.000000000000000000, -285.0000000000000000 ) ) ;
#7275 = ADVANCED_FACE ( 'NONE', ( #8363 ), #4181, .F. ) ;
#7276 = CARTESIAN_POINT ( 'NONE',  ( -0.4523805927985417030, -7.499149346347998346, -434.4772701732684936 ) ) ;
#7277 = CARTESIAN_POINT ( 'NONE',  ( -5.563766465756743607, -12.00000000000000000, -337.3048648817380126 ) ) ;
#7278 = DIRECTION ( 'NONE',  ( 0.000000000000000000, -1.000000000000000000, 0.000000000000000000 ) ) ;
#7279 = ORIENTED_EDGE ( 'NONE', *, *, #114, .T. ) ;
#7280 = CARTESIAN_POINT ( 'NONE',  ( -1.327715439883788706, -12.49239253839650843, 319.0000000000003979 ) ) ;
#7281 = ORIENTED_EDGE ( 'NONE', *, *, #7776, .T. ) ;
#7282 = CARTESIAN_POINT ( 'NONE',  ( -46.74071243416547361, -2.500000000000000000, -414.3237589990478114 ) ) ;
#7283 = VERTEX_POINT ( 'NONE', #2516 ) ;
#7284 = CARTESIAN_POINT ( 'NONE',  ( -8.778709539581399213, -8.123450746681353252, 315.0000000000000000 ) ) ;
#7285 = CARTESIAN_POINT ( 'NONE',  ( 18.21470573400001669, -4.474143576597000127, -302.4229045757450081 ) ) ;
#7286 = CIRCLE ( 'NONE', #921, 5.000000000000004441 ) ;
#7287 = CARTESIAN_POINT ( 'NONE',  ( -72.90663470102438737, -2.500000000000000444, -371.7168990826883714 ) ) ;
#7288 = VECTOR ( 'NONE', #8588, 1000.000000000000114 ) ;
#7289 = CARTESIAN_POINT ( 'NONE',  ( -50.24071243418999444, -2.500000000000000000, -414.3237589990000629 ) ) ;
#7290 = SURFACE_STYLE_USAGE ( .BOTH. , #8089 ) ;
#7291 = CARTESIAN_POINT ( 'NONE',  ( -13.72185241754999652, 8.618935511841003816, -302.4229045757450081 ) ) ;
#7292 = ADVANCED_FACE ( 'NONE', ( #5780 ), #1707, .F. ) ;
#7293 = DIRECTION ( 'NONE',  ( 0.000000000000000000, -1.000000000000000000, 0.000000000000000000 ) ) ;
#7294 = ORIENTED_EDGE ( 'NONE', *, *, #1550, .T. ) ;
#7295 = CARTESIAN_POINT ( 'NONE',  ( 10.40890489166000066, -7.434429060800999522, -315.0848619657999734 ) ) ;
#7296 = DIRECTION ( 'NONE',  ( 0.000000000000000000, 1.000000000000000000, -0.000000000000000000 ) ) ;
#7297 = VERTEX_POINT ( 'NONE', #4908 ) ;
#7298 = CARTESIAN_POINT ( 'NONE',  ( -16.73002466287002576, -6.274001814427998980, 189.9229057364800042 ) ) ;
#7299 = CARTESIAN_POINT ( 'NONE',  ( 17.02940347669788324, 6.570098831661549177, 190.9999999999996589 ) ) ;
#7300 = DIRECTION ( 'NONE',  ( 0.000000000000000000, 1.000000000000000000, 0.000000000000000000 ) ) ;
#7301 = AXIS2_PLACEMENT_3D ( 'NONE', #9283, #6912, #6809 ) ;
#7302 =( REPRESENTATION_RELATIONSHIP ('NONE','NONE', #8468, #1739 ) REPRESENTATION_RELATIONSHIP_WITH_TRANSFORMATION ( #3499 )SHAPE_REPRESENTATION_RELATIONSHIP( ) );
#7303 = CARTESIAN_POINT ( 'NONE',  ( -14.38384290288000145, -5.252906928686999599, 314.8616023057000461 ) ) ;
#7304 = CARTESIAN_POINT ( 'NONE',  ( -9.597846547914999249, 9.915773017694000657, 320.0000000000000000 ) ) ;
#7305 = CARTESIAN_POINT ( 'NONE',  ( -79.04021210711869116, -2.500000000000000000, -328.4066924704651456 ) ) ;
#7306 = CARTESIAN_POINT ( 'NONE',  ( -14.98500449093754483, -4.500000000000000888, -438.4247239981262396 ) ) ;
#7307 = CARTESIAN_POINT ( 'NONE',  ( 17.49999999911143433, -5.867334123717693473, -302.4999999999996021 ) ) ;
#7308 = DIRECTION ( 'NONE',  ( 0.000000000000000000, -1.000000000000000000, 0.000000000000000000 ) ) ;
#7309 = EDGE_CURVE ( 'NONE', #4372, #1489, #335, .T. ) ;
#7310 = ORIENTED_EDGE ( 'NONE', *, *, #2013, .F. ) ;
#7311 = CARTESIAN_POINT ( 'NONE',  ( -16.11962419174959393, -7.500000000000000000, -430.9361393731155658 ) ) ;
#7312 = ORIENTED_EDGE ( 'NONE', *, *, #1527, .T. ) ;
#7313 = B_SPLINE_CURVE_WITH_KNOTS ( 'NONE', 3,
 ( #1842, #5059, #7486, #3612, #5972, #10110, #2541, #5113, #1029, #4314, #180, #2597, #234, #9263, #5807, #1896, #9100, #2752, #6022, #3715, #3759, #3011, #385, #1343 ),
 .UNSPECIFIED., .F., .F.,
 ( 4, 1, 1, 1, 1, 1, 2, 2, 2, 1, 1, 1, 1, 1, 2, 2, 4 ),
 ( 0.000000000000000000, 0.1250000000000436873, 0.1875000000000811018, 0.2187500000000887901, 0.2343750000000931477, 0.2421875000000953404, 0.2460937500000959233, 0.2500000000000964784, 0.4999999999999881206, 0.6249999999999342748, 0.6874999999999298339, 0.7187499999999547029, 0.7343749999999963363, 0.7421875000000170974, 0.7460937500000278666, 0.7500000000000385247, 1.000000000000000000 ),
 .UNSPECIFIED. ) ;
#7314 = CARTESIAN_POINT ( 'NONE',  ( -33.34106825788445150, -7.500000000000000000, -439.6766126514281154 ) ) ;
#7315 = AXIS2_PLACEMENT_3D ( 'NONE', #6494, #8966, #4343 ) ;
#7316 = CARTESIAN_POINT ( 'NONE',  ( 11.80673610560780240, 6.814824988023822527, 315.0000000000000000 ) ) ;
#7317 = APPLICATION_PROTOCOL_DEFINITION ( 'draft international standard', 'automotive_design', 1998, #8451 ) ;
#7318 = CARTESIAN_POINT ( 'NONE',  ( -19.99984324442397465, -0.5882482212486090933, -303.4999999999997158 ) ) ;
#7319 = CARTESIAN_POINT ( 'NONE',  ( 17.56970546055000071, -0.4338786413876999926, -314.4150829855000211 ) ) ;
#7320 = CARTESIAN_POINT ( 'NONE',  ( -12.86189863199293093, -5.758762107780500017, -438.9337381413729418 ) ) ;
#7321 = CARTESIAN_POINT ( 'NONE',  ( 15.65693014362998348, 7.780815921226000853, 318.8802828394900644 ) ) ;
#7322 = DIRECTION ( 'NONE',  ( 0.000000000000000000, -1.000000000000000000, 0.000000000000000000 ) ) ;
#7323 = CARTESIAN_POINT ( 'NONE',  ( -1.584100026069928724, -2.658208447551997811, -435.2648446327503962 ) ) ;
#7324 = DIRECTION ( 'NONE',  ( -0.000000000000000000, 1.000000000000000000, 0.000000000000000000 ) ) ;
#7325 = CARTESIAN_POINT ( 'NONE',  ( 14.92964316144998627, 8.327009966606000901, -316.3802825947000201 ) ) ;
#7326 = DIRECTION ( 'NONE',  ( -0.000000000000000000, 1.000000000000000000, -0.000000000000000000 ) ) ;
#7327 = EDGE_CURVE ( 'NONE', #8080, #8626, #7710, .T. ) ;
#7328 = LINE ( 'NONE', #7274, #10088 ) ;
#7329 = CARTESIAN_POINT ( 'NONE',  ( -1.339266931960580331, -7.388578682852002366, -434.7178764703356251 ) ) ;
#7330 = DIRECTION ( 'NONE',  ( 0.000000000000000000, -1.000000000000000000, -0.000000000000000000 ) ) ;
#7331 = CARTESIAN_POINT ( 'NONE',  ( -16.63862268811586986, 3.034640078201995994, -314.5459747968306488 ) ) ;
#7332 = VERTEX_POINT ( 'NONE', #5652 ) ;
#7333 = CARTESIAN_POINT ( 'NONE',  ( -3.650011388878885210, -9.782272988550902326, -314.5118284007355669 ) ) ;
#7334 = ORIENTED_EDGE ( 'NONE', *, *, #7668, .T. ) ;
#7335 = CARTESIAN_POINT ( 'NONE',  ( -7.807700195763000117, 10.48319479899000051, -317.5000000000000000 ) ) ;
#7336 = ORIENTED_EDGE ( 'NONE', *, *, #2869, .F. ) ;
#7337 = CARTESIAN_POINT ( 'NONE',  ( 14.97309261602000419, -8.296494983500004139, -303.6197174156509391 ) ) ;
#7338 = CARTESIAN_POINT ( 'NONE',  ( 19.99999721132999753, -3.518697978483000342E-10, 319.0000000000000000 ) ) ;
#7339 = EDGE_CURVE ( 'NONE', #3077, #7180, #668, .T. ) ;
#7340 = DIRECTION ( 'NONE',  ( 0.000000000000000000, 1.000000000000000000, -0.000000000000000000 ) ) ;
#7341 = AXIS2_PLACEMENT_3D ( 'NONE', #8647, #4572, #7846 ) ;
#7342 = SHAPE_REPRESENTATION_RELATIONSHIP ( 'NONE' , 'NONE' ,  #1806, #453 ) ;
#7343 = CARTESIAN_POINT ( 'NONE',  ( 9.183684135703998663, 10.67340332910999834, -302.4229045757450081 ) ) ;
#7344 = CARTESIAN_POINT ( 'NONE',  ( -10.25126250535807770, -10.00000007971003058, 314.9999999999999432 ) ) ;
#7345 = ORIENTED_EDGE ( 'NONE', *, *, #3536, .F. ) ;
#7346 = CARTESIAN_POINT ( 'NONE',  ( -17.57772697299999720, 0.3191603157329000462, -314.4150829855000211 ) ) ;
#7347 = DIRECTION ( 'NONE',  ( 0.7784864941890657919, 0.000000000000000000, 0.6276613564377031551 ) ) ;
#7348 = EDGE_LOOP ( 'NONE', ( #9471, #8287, #6192, #6522 ) ) ;
#7349 = CARTESIAN_POINT ( 'NONE',  ( 13.77732760571000092, -8.580179748050001720, 189.9229057364800042 ) ) ;
#7350 = VECTOR ( 'NONE', #440, 1000.000000000000000 ) ;
#7351 = DIRECTION ( 'NONE',  ( 0.000000000000000000, 1.000000000000000000, 0.000000000000000000 ) ) ;
#7352 = CARTESIAN_POINT ( 'NONE',  ( 14.65054575295525119, 4.807282645526345100, -315.0000000000001137 ) ) ;
#7353 = DIRECTION ( 'NONE',  ( 1.000000000000000000, 0.000000000000000000, 0.000000000000000000 ) ) ;
#7354 = CARTESIAN_POINT ( 'NONE',  ( -15.23514566747999943, -4.427644513407000382, 314.8616023057000461 ) ) ;
#7355 = CARTESIAN_POINT ( 'NONE',  ( -0.6600210488075000104, 11.51366633668999917, 320.0000000000000000 ) ) ;
#7356 = DIRECTION ( 'NONE',  ( -0.8820010751365675583, 0.000000000000000000, -0.4712473909295827323 ) ) ;
#7357 = CARTESIAN_POINT ( 'NONE',  ( -14.75365836417945431, 8.451130538707893436, 319.0000000000005116 ) ) ;
#7358 = CARTESIAN_POINT ( 'NONE',  ( -20.40121062015000319, -2.500000000000000000, -430.0210166885000262 ) ) ;
#7359 = DIRECTION ( 'NONE',  ( 0.4712473909295827323, 0.000000000000000000, -0.8820010751365675583 ) ) ;
#7360 = ORIENTED_EDGE ( 'NONE', *, *, #9425, .F. ) ;
#7361 = CARTESIAN_POINT ( 'NONE',  ( -13.57573464316000056, 3.225916527208000151, -285.0000000000000000 ) ) ;
#7362 = ORIENTED_EDGE ( 'NONE', *, *, #8616, .F. ) ;
#7363 = DIRECTION ( 'NONE',  ( -0.7880107536076077501, 0.000000000000000000, -0.6156614753245244209 ) ) ;
#7364 = DIRECTION ( 'NONE',  ( 0.9958031466069979798, 0.000000000000000000, 0.09152099872489198595 ) ) ;
#7365 = CONTEXT_DEPENDENT_SHAPE_REPRESENTATION ( #102, #2782 ) ;
#7366 = CARTESIAN_POINT ( 'NONE',  ( 7.927914882803702490, -11.48831374418035089, -303.4999999999996589 ) ) ;
#7367 = AXIS2_PLACEMENT_3D ( 'NONE', #10357, #9500, #4499 ) ;
#7368 = LINE ( 'NONE', #3932, #7975 ) ;
#7369 = AXIS2_PLACEMENT_3D ( 'NONE', #2435, #7326, #5705 ) ;
#7370 = CARTESIAN_POINT ( 'NONE',  ( 10.00000000000000000, -2.500000000000000000, -272.5000000000000000 ) ) ;
#7371 = CARTESIAN_POINT ( 'NONE',  ( -5.530027647682731917, -6.775927878003381366, -436.8017055862294455 ) ) ;
#7372 = CARTESIAN_POINT ( 'NONE',  ( -14.93900900976164969, -5.907301249192538961, -438.6122981656100137 ) ) ;
#7373 = CARTESIAN_POINT ( 'NONE',  ( -0.6109814867824735485, -2.478111245608000779, -434.8347466770483152 ) ) ;
#7374 = ORIENTED_EDGE ( 'NONE', *, *, #6882, .F. ) ;
#7375 = CARTESIAN_POINT ( 'NONE',  ( 4.990336260259995882, 12.19640393417999036, -317.0792622552969533 ) ) ;
#7376 = CARTESIAN_POINT ( 'NONE',  ( -30.41084982323499730, -7.500000000000000000, -460.5301199443746327 ) ) ;
#7377 = CIRCLE ( 'NONE', #2745, 1.000009933063999545 ) ;
#7378 = EDGE_CURVE ( 'NONE', #6469, #9547, #9692, .T. ) ;
#7379 = ORIENTED_EDGE ( 'NONE', *, *, #8075, .T. ) ;
#7380 = CARTESIAN_POINT ( 'NONE',  ( -3.142739053800999827, -11.35686622240999810, 320.0000000000000000 ) ) ;
#7381 = SHAPE_REPRESENTATION ( 'Hinge Pin', ( #2817 ), #3838 ) ;
#7382 = CARTESIAN_POINT ( 'NONE',  ( -1.245518217540318773, -7.397396954862998086, -434.6795757337810642 ) ) ;
#7383 = DIRECTION ( 'NONE',  ( -0.8820010751365716661, 0.000000000000000000, -0.4712473909295749053 ) ) ;
#7384 = CARTESIAN_POINT ( 'NONE',  ( 15.48916725177958398, -3.890278845006962083, -315.0000000000000000 ) ) ;
#7385 = ORIENTED_EDGE ( 'NONE', *, *, #4237, .F. ) ;
#7386 = CARTESIAN_POINT ( 'NONE',  ( -15.67978886374999803, 4.575336738469999887, -315.0000000000001137 ) ) ;
#7387 = ORIENTED_EDGE ( 'NONE', *, *, #7077, .T. ) ;
#7388 = CARTESIAN_POINT ( 'NONE',  ( -10.00000000000000000, 2.500000000000000000, -315.0000000000000000 ) ) ;
#7389 = VERTEX_POINT ( 'NONE', #7277 ) ;
#7390 = CARTESIAN_POINT ( 'NONE',  ( -15.91674550148000122, -7.581266318323002906, -303.6197174156509391 ) ) ;
#7391 = ADVANCED_FACE ( 'NONE', ( #6465 ), #1685, .T. ) ;
#7392 = DIRECTION ( 'NONE',  ( 0.000000000000000000, 1.000000000000000000, -0.000000000000000000 ) ) ;
#7393 = CYLINDRICAL_SURFACE ( 'NONE', #3338, 0.5000000000000074385 ) ;
#7394 = AXIS2_PLACEMENT_3D ( 'NONE', #10573, #1654, #4129 ) ;
#7395 = VECTOR ( 'NONE', #8987, 1000.000000000000000 ) ;
#7396 = CARTESIAN_POINT ( 'NONE',  ( -11.71875184657000091, 10.13482718352000944, -303.6197174156509391 ) ) ;
#7397 = ORIENTED_EDGE ( 'NONE', *, *, #2353, .T. ) ;
#7398 = CARTESIAN_POINT ( 'NONE',  ( -16.39086977655999888, -2.839079766962000040, -314.8616023057000461 ) ) ;
#7399 = CARTESIAN_POINT ( 'NONE',  ( 1.399293614871181202, -2.500000000000000000, -408.6664516090914390 ) ) ;
#7400 = ORIENTED_EDGE ( 'NONE', *, *, #3321, .T. ) ;
#7401 = CARTESIAN_POINT ( 'NONE',  ( 14.03700484701000484, -9.005201968871000773, 190.4207385301700128 ) ) ;
#7402 = CARTESIAN_POINT ( 'NONE',  ( -17.50000000000107292, -0.7437989020622546299, -314.4944826805095772 ) ) ;
#7403 = CARTESIAN_POINT ( 'NONE',  ( 15.63394123731325358, 3.714777356940325070, -314.9999999999999432 ) ) ;
#7404 = DIRECTION ( 'NONE',  ( 0.000000000000000000, 0.000000000000000000, -1.000000000000000000 ) ) ;
#7405 = VECTOR ( 'NONE', #7322, 1000.000000000000000 ) ;
#7406 = CARTESIAN_POINT ( 'NONE',  ( 8.620760283086999820, -8.357092890497000326, 314.8616023057000461 ) ) ;
#7407 = DIRECTION ( 'NONE',  ( 0.000000000000000000, -1.000000000000000000, 0.000000000000000000 ) ) ;
#7408 = CARTESIAN_POINT ( 'NONE',  ( 2.538616493050997569, -11.99586634586999523, 320.0770942683900557 ) ) ;
#7409 = CARTESIAN_POINT ( 'NONE',  ( 19.14895805910628468, 3.641352296147347012, 319.0000000000005116 ) ) ;
#7410 = CARTESIAN_POINT ( 'NONE',  ( 15.92130416703352580, 7.586839038430810866, -303.5000000000000000 ) ) ;
#7411 = CARTESIAN_POINT ( 'NONE',  ( 17.34089965840999881, 0.6440164457022999889, 314.6383426456000052 ) ) ;
#7412 = VERTEX_POINT ( 'NONE', #4959 ) ;
#7413 = DIRECTION ( 'NONE',  ( 0.000000000000000000, -1.000000000000000000, 0.000000000000000000 ) ) ;
#7414 = ORIENTED_EDGE ( 'NONE', *, *, #6677, .F. ) ;
#7415 = AXIS2_PLACEMENT_3D ( 'NONE', #3343, #7863, #5751 ) ;
#7416 = CARTESIAN_POINT ( 'NONE',  ( -0.8407996126558667793, -7.500000000000000888, -352.5919046247526580 ) ) ;
#7417 = CARTESIAN_POINT ( 'NONE',  ( -19.00000000000000000, 0.000000000000000000, -302.5000000001010108 ) ) ;
#7418 = ITEM_DEFINED_TRANSFORMATION ( 'NONE', 'NONE', #8855,  #2817 ) ;
#7419 = FACE_OUTER_BOUND ( 'NONE', #9833, .T. ) ;
#7420 = ORIENTED_EDGE ( 'NONE', *, *, #5706, .T. ) ;
#7421 = CARTESIAN_POINT ( 'NONE',  ( -1.638209378284813722, -2.561752193325623317, -434.6868264169996223 ) ) ;
#7422 = DIRECTION ( 'NONE',  ( 0.000000000000000000, -1.000000000000000000, 0.000000000000000000 ) ) ;
#7423 = EDGE_CURVE ( 'NONE', #3371, #7412, #9946, .T. ) ;
#7424 = CIRCLE ( 'NONE', #6208, 3.500000000000020428 ) ;
#7425 =( NAMED_UNIT ( * ) SI_UNIT ( $, .STERADIAN. ) SOLID_ANGLE_UNIT ( ) );
#7426 = FILL_AREA_STYLE_COLOUR ( '', #5158 ) ;
#7427 = AXIS2_PLACEMENT_3D ( 'NONE', #6179, #10273, #2910 ) ;
#7428 = CARTESIAN_POINT ( 'NONE',  ( -14.79012398734008293, 1.483731117706880154, -284.9999999999999432 ) ) ;
#7429 = ORIENTED_EDGE ( 'NONE', *, *, #3774, .F. ) ;
#7430 = CARTESIAN_POINT ( 'NONE',  ( -20.01697452336999561, 0.3413909698088000710, -316.3802825947000201 ) ) ;
#7431 = DIRECTION ( 'NONE',  ( 0.000000000000000000, -1.000000000000000000, 0.000000000000000000 ) ) ;
#7432 = CARTESIAN_POINT ( 'NONE',  ( -0.1421619115827766622, -7.644091901224001617, -434.3437170732802315 ) ) ;
#7433 = VECTOR ( 'NONE', #4587, 1000.000000000000000 ) ;
#7434 = UNCERTAINTY_MEASURE_WITH_UNIT (LENGTH_MEASURE( 1.000000000000000082E-05 ), #4796, 'distance_accuracy_value', 'NONE');
#7435 = CARTESIAN_POINT ( 'NONE',  ( 18.99997865338999858, -1.260542273207000211E-06, -316.5000000000000000 ) ) ;
#7436 = CARTESIAN_POINT ( 'NONE',  ( 11.78094678683302554, -6.828785851005064522, -315.0000000000000568 ) ) ;
#7437 = ORIENTED_EDGE ( 'NONE', *, *, #3985, .T. ) ;
#7438 = CARTESIAN_POINT ( 'NONE',  ( -1.831806507035719234, -9.955740905498862148, -314.5031779949863449 ) ) ;
#7439 = ORIENTED_EDGE ( 'NONE', *, *, #4899, .F. ) ;
#7440 = CARTESIAN_POINT ( 'NONE',  ( -2.034678270035999770, 11.44985799554000039, -317.5000000000000000 ) ) ;
#7441 = ORIENTED_EDGE ( 'NONE', *, *, #8921, .T. ) ;
#7442 = CARTESIAN_POINT ( 'NONE',  ( -8.030503796230000546, -11.45221762926000153, -303.6197174156509391 ) ) ;
#7443 = APPLICATION_CONTEXT ( 'automotive_design' ) ;
#7444 = CARTESIAN_POINT ( 'NONE',  ( 15.00000000000000000, -0.4945770392355999800, 315.0000000000000000 ) ) ;
#7445 = CARTESIAN_POINT ( 'NONE',  ( -16.88084019735002173, 6.719348373024005561, -303.6197174156509391 ) ) ;
#7446 = CARTESIAN_POINT ( 'NONE',  ( -17.50000000000000000, -3.147917160613439321E-08, 314.4997059534069308 ) ) ;
#7447 = ORIENTED_EDGE ( 'NONE', *, *, #4779, .F. ) ;
#7448 = DIRECTION ( 'NONE',  ( 0.8820010751365653379, 0.000000000000000000, 0.4712473909295871732 ) ) ;
#7449 = DIRECTION ( 'NONE',  ( 0.1071946444232959594, 0.000000000000000000, -0.9942380540931649024 ) ) ;
#7450 = EDGE_LOOP ( 'NONE', ( #3682, #8862, #4324, #4214 ) ) ;
#7451 = CARTESIAN_POINT ( 'NONE',  ( 19.12235363464000670, -3.679291565416002108, 191.1197171614399792 ) ) ;
#7452 = LINE ( 'NONE', #1757, #2644 ) ;
#7453 = DIRECTION ( 'NONE',  ( 0.000000000000000000, 0.000000000000000000, -1.000000000000000000 ) ) ;
#7454 = DIRECTION ( 'NONE',  ( 0.000000000000000000, 1.000000000000000000, 0.000000000000000000 ) ) ;
#7455 = CARTESIAN_POINT ( 'NONE',  ( 16.39938580555998726, 7.272241081627004000, 190.4207385301700128 ) ) ;
#7456 = AXIS2_PLACEMENT_3D ( 'NONE', #8058, #6447, #703 ) ;
#7457 = VECTOR ( 'NONE', #6513, 1000.000000000000114 ) ;
#7458 = ORIENTED_EDGE ( 'NONE', *, *, #8317, .T. ) ;
#7459 = CARTESIAN_POINT ( 'NONE',  ( 17.56954514911999965, 0.4333932196220000033, 314.4150829855000211 ) ) ;
#7460 = SURFACE_STYLE_USAGE ( .BOTH. , #5255 ) ;
#7461 = CARTESIAN_POINT ( 'NONE',  ( 15.00000000000000000, 0.000000000000000000, -285.0000000000000000 ) ) ;
#7462 = CARTESIAN_POINT ( 'NONE',  ( 15.57034186525998543, -6.406527364046002759, 319.9928079742500131 ) ) ;
#7463 = CARTESIAN_POINT ( 'NONE',  ( -12.89381003144900184, 6.798165335629914097, 314.4999421354863216 ) ) ;
#7464 = CARTESIAN_POINT ( 'NONE',  ( 17.57772697299999720, -0.3191603157329000462, 314.4150829855000211 ) ) ;
#7465 = ORIENTED_EDGE ( 'NONE', *, *, #5221, .F. ) ;
#7466 = CARTESIAN_POINT ( 'NONE',  ( 17.62182611535273935, -5.928443937941890063, 190.9999999999995737 ) ) ;
#7467 = ORIENTED_EDGE ( 'NONE', *, *, #6253, .T. ) ;
#7468 = ORIENTED_EDGE ( 'NONE', *, *, #8088, .T. ) ;
#7469 = AXIS2_PLACEMENT_3D ( 'NONE', #2025, #7764, #7870 ) ;
#7470 = ADVANCED_FACE ( 'NONE', ( #10490, #4103 ), #3192, .T. ) ;
#7471 = EDGE_CURVE ( 'NONE', #4813, #1205, #3760, .T. ) ;
#7472 = CARTESIAN_POINT ( 'NONE',  ( -12.95168464415343834, -4.250977063078799745, -439.0697824306216717 ) ) ;
#7473 = CARTESIAN_POINT ( 'NONE',  ( -11.69610966801475449, 6.874282731906364852, 315.0000000000000000 ) ) ;
#7474 = FACE_OUTER_BOUND ( 'NONE', #4875, .T. ) ;
#7475 = ORIENTED_EDGE ( 'NONE', *, *, #1952, .F. ) ;
#7476 =( GEOMETRIC_REPRESENTATION_CONTEXT ( 3 ) GLOBAL_UNCERTAINTY_ASSIGNED_CONTEXT ( ( #2705 ) ) GLOBAL_UNIT_ASSIGNED_CONTEXT ( ( #4488, #6766, #7671 ) ) REPRESENTATION_CONTEXT ( 'NONE', 'WORKASPACE' ) );
#7477 = CARTESIAN_POINT ( 'NONE',  ( 7.649658656166000270, -10.52693506402999901, -302.5000000000000000 ) ) ;
#7478 = CARTESIAN_POINT ( 'NONE',  ( -101.0297452788102817, -2.500000000000000000, -342.4231267849074811 ) ) ;
#7479 = CARTESIAN_POINT ( 'NONE',  ( 0.6643694614233000006, 11.51357945830000062, 190.0000000000000000 ) ) ;
#7480 = LINE ( 'NONE', #10593, #10148 ) ;
#7481 = CARTESIAN_POINT ( 'NONE',  ( -0.4215672289900458392, -2.433748306090999236, -434.7071814881026057 ) ) ;
#7482 = CARTESIAN_POINT ( 'NONE',  ( 17.49999012170142620, -5.867339742191236773, 190.0000000000003695 ) ) ;
#7483 = CARTESIAN_POINT ( 'NONE',  ( -2.060812052271002059, 12.52766984582000021, -317.0792622552969533 ) ) ;
#7484 = AXIS2_PLACEMENT_3D ( 'NONE', #5425, #1240, #8701 ) ;
#7485 = EDGE_CURVE ( 'NONE', #5506, #10253, #9637, .T. ) ;
#7486 = CARTESIAN_POINT ( 'NONE',  ( 8.989791091710285897, -4.160326409263540803, -525.4993780678859139 ) ) ;
#7487 = DIRECTION ( 'NONE',  ( 8.659560562355927562E-17, -0.7071067811864661934, 0.7071067811866287300 ) ) ;
#7488 = LINE ( 'NONE', #5922, #796 ) ;
#7489 = CARTESIAN_POINT ( 'NONE',  ( 16.37160231057345428, -2.539265572400264404, -315.0000000000000000 ) ) ;
#7490 = ORIENTED_EDGE ( 'NONE', *, *, #10284, .F. ) ;
#7491 = CARTESIAN_POINT ( 'NONE',  ( 8.988119689606872242, -8.550792887852699309, -314.5455502384735951 ) ) ;
#7492 = VERTEX_POINT ( 'NONE', #4157 ) ;
#7493 = CARTESIAN_POINT ( 'NONE',  ( 3.336936413097000287, 11.33398029193999967, -317.5000000000000000 ) ) ;
#7494 = ORIENTED_EDGE ( 'NONE', *, *, #8843, .F. ) ;
#7495 = CARTESIAN_POINT ( 'NONE',  ( -9.312701725069002734, -11.06649994634999246, -303.6197174156509391 ) ) ;
#7496 = CARTESIAN_POINT ( 'NONE',  ( 18.29581373626999508, -2.889895519923001643, -317.4928077629770087 ) ) ;
#7497 = CARTESIAN_POINT ( 'NONE',  ( -17.12432750374000179, -0.4000877216259000058, -314.8616023057000461 ) ) ;
#7498 = ADVANCED_FACE ( 'NONE', ( #720, #3995, #10551 ), #4054, .F. ) ;
#7499 = CARTESIAN_POINT ( 'NONE',  ( 19.29864983862999850, 3.387441872937999143, -303.6197174156509391 ) ) ;
#7500 = DIRECTION ( 'NONE',  ( 0.6276613564377032661, 0.000000000000000000, -0.7784864941890657919 ) ) ;
#7501 = ORIENTED_EDGE ( 'NONE', *, *, #9391, .F. ) ;
#7502 = CARTESIAN_POINT ( 'NONE',  ( -0.5933647373784489698, -7.500000025448000152, -434.1978076166600431 ) ) ;
#7503 = CARTESIAN_POINT ( 'NONE',  ( -15.16362200326591569, -3.250000000000000444, -437.6963039377973246 ) ) ;
#7504 = ORIENTED_EDGE ( 'NONE', *, *, #1909, .F. ) ;
#7505 = CARTESIAN_POINT ( 'NONE',  ( 19.49006540358000805, -2.831553480999998929, 191.1197171614399792 ) ) ;
#7506 = CARTESIAN_POINT ( 'NONE',  ( 8.037373804805000077, -9.179324345868998591, -314.4944826805095772 ) ) ;
#7507 = CARTESIAN_POINT ( 'NONE',  ( 15.40306756913855146, 3.994766537461135858, -314.9999999999998863 ) ) ;
#7508 = DIRECTION ( 'NONE',  ( -0.6276613564377034882, 0.000000000000000000, 0.7784864941890656809 ) ) ;
#7509 = CARTESIAN_POINT ( 'NONE',  ( -10.15702342499999844, 10.85948264422000165, 190.4207385301700128 ) ) ;
#7510 = EDGE_CURVE ( 'NONE', #7297, #9430, #8221, .T. ) ;
#7511 = CARTESIAN_POINT ( 'NONE',  ( 16.90171868104999930, 0.3834349726278000192, 315.0848619657999734 ) ) ;
#7512 = CARTESIAN_POINT ( 'NONE',  ( 10.00000000000000000, -2.500000000000000000, -317.5000000000000000 ) ) ;
#7513 = CARTESIAN_POINT ( 'NONE',  ( -19.56036306585002293, 0.5267516669946002983, 320.0770942683900557 ) ) ;
#7514 = CARTESIAN_POINT ( 'NONE',  ( -18.02719435607597021, -7.500000000000000888, -431.8467903975401896 ) ) ;
#7515 = CARTESIAN_POINT ( 'NONE',  ( 16.07469914181999826, 3.754035329064000059, 314.6383426456000052 ) ) ;
#7516 = ORIENTED_EDGE ( 'NONE', *, *, #8738, .T. ) ;
#7517 = DIRECTION ( 'NONE',  ( 0.000000000000000000, -1.000000000000000000, 0.000000000000000000 ) ) ;
#7518 = CARTESIAN_POINT ( 'NONE',  ( -11.00353245304999739, 10.53087951318999593, 319.5792614743400009 ) ) ;
#7519 = VERTEX_POINT ( 'NONE', #9747 ) ;
#7520 = EDGE_CURVE ( 'NONE', #1584, #2824, #10449, .T. ) ;
#7521 = EDGE_CURVE ( 'NONE', #3286, #2509, #10122, .T. ) ;
#7522 = DIRECTION ( 'NONE',  ( -0.9627072963110285819, 0.1321637200909012433, -0.2360665429942227778 ) ) ;
#7523 = CARTESIAN_POINT ( 'NONE',  ( -12.16656789651012005, 6.621481216618937182, 314.9999999999999432 ) ) ;
#7524 = ITEM_DEFINED_TRANSFORMATION ( 'NONE', 'NONE', #7484,  #2817 ) ;
#7525 = DIRECTION ( 'NONE',  ( 6.938893903907222067E-14, -1.000000000000000000, -1.110223024625155531E-13 ) ) ;
#7526 = VERTEX_POINT ( 'NONE', #9802 ) ;
#7527 = CARTESIAN_POINT ( 'NONE',  ( 19.00000000000000000, 0.000000000000000000, -302.5000000001010108 ) ) ;
#7528 = CARTESIAN_POINT ( 'NONE',  ( -7.893353328029269811, -6.500255900689999145, -436.7904933931527580 ) ) ;
#7529 = EDGE_CURVE ( 'NONE', #5593, #8113, #8495, .T. ) ;
#7530 = CARTESIAN_POINT ( 'NONE',  ( 17.50000000000002487, 1.995060298004523415E-08, 314.4999385900306947 ) ) ;
#7531 = FACE_OUTER_BOUND ( 'NONE', #6645, .T. ) ;
#7532 = EDGE_LOOP ( 'NONE', ( #8527, #4861, #6412, #8359 ) ) ;
#7533 = DIRECTION ( 'NONE',  ( -0.9902680687415799099, 0.000000000000000000, -0.1391731009599969648 ) ) ;
#7534 = DIRECTION ( 'NONE',  ( -1.000000000000000000, 0.000000000000000000, 0.000000000000000000 ) ) ;
#7535 = DIRECTION ( 'NONE',  ( 0.000000000000000000, -1.000000000000000000, 0.000000000000000000 ) ) ;
#7536 = UNCERTAINTY_MEASURE_WITH_UNIT (LENGTH_MEASURE( 1.000000000000000082E-05 ), #4615, 'distance_accuracy_value', 'NONE');
#7537 = CARTESIAN_POINT ( 'NONE',  ( -77.77979771402830522, -2.500000000000000000, -385.9384419754180158 ) ) ;
#7538 = CARTESIAN_POINT ( 'NONE',  ( 11.80659750965543608, -6.814906413124091067, -314.9999999999999432 ) ) ;
#7539 = ORIENTED_EDGE ( 'NONE', *, *, #4174, .T. ) ;
#7540 = CARTESIAN_POINT ( 'NONE',  ( 12.32405526929588113, -7.045528031251313550, -314.5741454722275421 ) ) ;
#7541 = CARTESIAN_POINT ( 'NONE',  ( -45.24937426871918689, -7.500000000000000000, -448.9804009737068213 ) ) ;
#7542 = ORIENTED_EDGE ( 'NONE', *, *, #507, .T. ) ;
#7543 = CARTESIAN_POINT ( 'NONE',  ( -27.18445350464674348, -7.656480000000000175, -447.5567201875090291 ) ) ;
#7544 = ORIENTED_EDGE ( 'NONE', *, *, #867, .T. ) ;
#7545 = CARTESIAN_POINT ( 'NONE',  ( 3.435942420224999072, -12.40730057411998821, -302.9207377450070453 ) ) ;
#7546 = AXIS2_PLACEMENT_3D ( 'NONE', #4234, #9180, #1818 ) ;
#7547 = CIRCLE ( 'NONE', #7711, 20.50000098877001165 ) ;
#7548 = CARTESIAN_POINT ( 'NONE',  ( 16.09890757810000750, -5.925814185855000638, -317.4928077629770087 ) ) ;
#7549 = DIRECTION ( 'NONE',  ( 0.9921831154218024862, -0.000000000000000000, 0.1247904863035890766 ) ) ;
#7550 = DIRECTION ( 'NONE',  ( 0.000000000000000000, 0.000000000000000000, 1.000000000000000000 ) ) ;
#7551 = AXIS2_PLACEMENT_3D ( 'NONE', #3751, #7041, #4455 ) ;
#7552 = CARTESIAN_POINT ( 'NONE',  ( 19.86714287764001696, 1.744094218545000352, -303.6197174156520759 ) ) ;
#7553 = DIRECTION ( 'NONE',  ( -0.8820010751365675583, 0.000000000000000000, -0.4712473909295827323 ) ) ;
#7554 = ORIENTED_EDGE ( 'NONE', *, *, #1217, .T. ) ;
#7555 = CARTESIAN_POINT ( 'NONE',  ( -17.14610219660000112, -0.04370646908745000336, -314.8616023057000461 ) ) ;
#7556 = CARTESIAN_POINT ( 'NONE',  ( -18.99984306468000028, 0.5551939808346000316, -302.5000000001010108 ) ) ;
#7557 = ORIENTED_EDGE ( 'NONE', *, *, #5245, .T. ) ;
#7558 = CARTESIAN_POINT ( 'NONE',  ( -19.86706274963002983, -1.898735342979001484, 190.4207385301700128 ) ) ;
#7559 = CARTESIAN_POINT ( 'NONE',  ( -8.037373804805000077, -9.179324345868998591, -315.0000000000001137 ) ) ;
#7560 = CARTESIAN_POINT ( 'NONE',  ( -72.90663470102438737, -8.000000000000000000, -371.7168990826883714 ) ) ;
#7561 = CARTESIAN_POINT ( 'NONE',  ( 18.27235334878999851, 5.234940180598000481, 190.4207385301700128 ) ) ;
#7562 = TOROIDAL_SURFACE ( 'NONE', #2923, 15.50000000000000000, 0.5000000000000000000 ) ;
#7563 = VERTEX_POINT ( 'NONE', #9856 ) ;
#7564 = CARTESIAN_POINT ( 'NONE',  ( 16.60805916514000202, -2.908391789136000050, 314.6383426456000052 ) ) ;
#7565 = CYLINDRICAL_SURFACE ( 'NONE', #8444, 5.000000000000004441 ) ;
#7566 = CARTESIAN_POINT ( 'NONE',  ( -3.163121738623003054, -11.93735872977999968, 320.0770942683900557 ) ) ;
#7567 = CARTESIAN_POINT ( 'NONE',  ( -14.98500449093754483, -3.250000000000000444, -438.4247239981262396 ) ) ;
#7568 = CARTESIAN_POINT ( 'NONE',  ( -15.96459840556375376, 7.551217265629138531, -303.5000000000000000 ) ) ;
#7569 = CARTESIAN_POINT ( 'NONE',  ( 13.44085293541000148, 6.266915263066000108, 314.6383426456000052 ) ) ;
#7570 = EDGE_LOOP ( 'NONE', ( #5283, #4230, #67, #7504 ) ) ;
#7571 = DIRECTION ( 'NONE',  ( 0.000000000000000000, -1.000000000000000000, 0.000000000000000000 ) ) ;
#7572 = CARTESIAN_POINT ( 'NONE',  ( 16.37943014210002346, 7.176468652514003566, 318.8802828394900644 ) ) ;
#7573 = DIRECTION ( 'NONE',  ( 0.000000000000000000, 1.000000000000000000, 0.000000000000000000 ) ) ;
#7574 = CARTESIAN_POINT ( 'NONE',  ( -8.616673968646825443, 8.177724119443702477, 315.0000000000000000 ) ) ;
#7575 = CONTEXT_DEPENDENT_SHAPE_REPRESENTATION ( #1665, #6995 ) ;
#7576 = CARTESIAN_POINT ( 'NONE',  ( -39.23786858994942151, -8.000000000000000000, -387.8670522075712483 ) ) ;
#7577 = EDGE_LOOP ( 'NONE', ( #9160, #5510, #9872, #6031 ) ) ;
#7578 = CARTESIAN_POINT ( 'NONE',  ( -1.813125407131493949, -2.572135581867000198, -434.7536649739391237 ) ) ;
#7579 = DIRECTION ( 'NONE',  ( -0.8820010751365678914, 0.000000000000000000, -0.4712473909295818442 ) ) ;
#7580 = CARTESIAN_POINT ( 'NONE',  ( 4.353497780899999725, 11.20674699699000065, 190.0000000000000000 ) ) ;
#7581 = CARTESIAN_POINT ( 'NONE',  ( -16.24410010525431503, 2.791089382272745834, -315.0000000000000000 ) ) ;
#7582 = CARTESIAN_POINT ( 'NONE',  ( -1.873948611767810357, -2.500000000000000000, -349.2478646809746579 ) ) ;
#7584 = CARTESIAN_POINT ( 'NONE',  ( -12.57201637590000942, 8.467554047266999007, 190.0071920248299477 ) ) ;
#7583 = AXIS2_PLACEMENT_3D ( 'NONE', #10417, #3059, #8805 ) ;
#7585 = PLANE ( 'NONE',  #2539 ) ;
#7586 = EDGE_CURVE ( 'NONE', #5350, #726, #6516, .T. ) ;
#7587 = CARTESIAN_POINT ( 'NONE',  ( 7.750957818532088872, -5.672096822788666337, -525.7290262469028903 ) ) ;
#7588 = AXIS2_PLACEMENT_3D ( 'NONE', #5814, #9807, #931 ) ;
#7589 = DIRECTION ( 'NONE',  ( 0.000000000000000000, -1.000000000000000000, 0.000000000000000000 ) ) ;
#7590 = CARTESIAN_POINT ( 'NONE',  ( -4.298300662841374020, -9.188610398197571527, -315.0000000000000568 ) ) ;
#7591 = EDGE_CURVE ( 'NONE', #9045, #2333, #1886, .T. ) ;
#7592 = VECTOR ( 'NONE', #3660, 1000.000000000000000 ) ;
#7593 = VERTEX_POINT ( 'NONE', #10066 ) ;
#7594 = DIRECTION ( 'NONE',  ( -0.7880107536076077501, 0.000000000000000000, -0.6156614753245244209 ) ) ;
#7595 = EDGE_LOOP ( 'NONE', ( #2404, #647, #10557, #3407 ) ) ;
#7596 = DIRECTION ( 'NONE',  ( 0.000000000000000000, 1.000000000000000000, 0.000000000000000000 ) ) ;
#7597 = ORIENTED_EDGE ( 'NONE', *, *, #3133, .F. ) ;
#7598 = LINE ( 'NONE', #2059, #1269 ) ;
#7599 = CARTESIAN_POINT ( 'NONE',  ( 0.2281161656705998908, -11.39695712172000164, -317.4928077629770087 ) ) ;
#7600 = EDGE_CURVE ( 'NONE', #8108, #215, #2706, .T. ) ;
#7601 = VECTOR ( 'NONE', #1474, 1000.000000000000000 ) ;
#7602 = CARTESIAN_POINT ( 'NONE',  ( -17.43193685618000188, 1.405086463480999859, -314.4150829855000211 ) ) ;
#7603 = CARTESIAN_POINT ( 'NONE',  ( -19.97270637197000909, -0.5553832019671004483, -303.6197174156509391 ) ) ;
#7604 = CARTESIAN_POINT ( 'NONE',  ( 2.881524480432390771E-09, -9.999999999999998224, 315.0000000000000000 ) ) ;
#7605 = VERTEX_POINT ( 'NONE', #5006 ) ;
#7606 = CARTESIAN_POINT ( 'NONE',  ( -0.6643694614234000317, -11.51357945830000062, 190.0000000000000000 ) ) ;
#7607 = CARTESIAN_POINT ( 'NONE',  ( -16.15280651819000113, 6.039793344733999980, -302.5000000000000000 ) ) ;
#7608 = ORIENTED_EDGE ( 'NONE', *, *, #10479, .T. ) ;
#7609 = CARTESIAN_POINT ( 'NONE',  ( 7.802724030307999215, -11.60041405728999919, 190.4207385301700128 ) ) ;
#7610 = B_SPLINE_CURVE_WITH_KNOTS ( 'NONE', 1,
 ( #10509, #2240 ),
 .UNSPECIFIED., .F., .F.,
 ( 2, 2 ),
 ( 0.01907785912498438652, 0.8020667992272817459 ),
 .UNSPECIFIED. ) ;
#7611 = CARTESIAN_POINT ( 'NONE',  ( 17.50000000000125056, 1.380497925828168986E-12, -315.0000000000001705 ) ) ;
#7612 = CARTESIAN_POINT ( 'NONE',  ( 15.25170542629001602, -6.686182281419003282, -302.5071922382879279 ) ) ;
#7613 = CARTESIAN_POINT ( 'NONE',  ( -13.14174346518001535, 9.520659322650999457, 190.4207385301700128 ) ) ;
#7614 = ORIENTED_EDGE ( 'NONE', *, *, #2317, .F. ) ;
#7615 = EDGE_CURVE ( 'NONE', #3896, #2293, #5304, .T. ) ;
#7616 = CARTESIAN_POINT ( 'NONE',  ( 10.67587555525000020, -8.049811041411000900, 314.4150829855000211 ) ) ;
#7617 = VECTOR ( 'NONE', #6475, 1000.000000000000000 ) ;
#7618 = DIRECTION ( 'NONE',  ( -0.000000000000000000, 1.000000000000000000, 0.000000000000000000 ) ) ;
#7619 = CARTESIAN_POINT ( 'NONE',  ( 18.69275906597000869, -1.650694058049998469, 319.9928079742500131 ) ) ;
#7620 = CARTESIAN_POINT ( 'NONE',  ( -7.551446853019275984, 9.031194155076960328, 314.4999434017205431 ) ) ;
#7621 = CARTESIAN_POINT ( 'NONE',  ( -12.85811403544582454, 9.588400772462147614, -303.5000000000000000 ) ) ;
#7622 = CARTESIAN_POINT ( 'NONE',  ( 17.35477687787999912, -0.3068793820639000303, 314.6383426456000052 ) ) ;
#7623 = ORIENTED_EDGE ( 'NONE', *, *, #6017, .F. ) ;
#7624 = CARTESIAN_POINT ( 'NONE',  ( 14.83495203015046648, -8.394818437327874250, 190.9999999999995737 ) ) ;
#7625 = CARTESIAN_POINT ( 'NONE',  ( 17.71262672283002360, 5.941112223585997221, 319.5792614743400009 ) ) ;
#7626 = AXIS2_PLACEMENT_3D ( 'NONE', #10263, #8583, #9408 ) ;
#7627 = CARTESIAN_POINT ( 'NONE',  ( -13.35722287852525270, -3.136587239007000871, -438.0342749280858925 ) ) ;
#7628 = CARTESIAN_POINT ( 'NONE',  ( 8.021995032228604217, 8.375907102466543463, 315.0000000000000568 ) ) ;
#7629 = EDGE_CURVE ( 'NONE', #4350, #4635, #2226, .T. ) ;
#7630 = DIRECTION ( 'NONE',  ( 0.000000000000000000, -1.000000000000000000, 0.000000000000000000 ) ) ;
#7631 = ORIENTED_EDGE ( 'NONE', *, *, #4776, .T. ) ;
#7632 = CARTESIAN_POINT ( 'NONE',  ( -5.145495120689000501, -11.07694361959999974, -302.5000000000000000 ) ) ;
#7633 = CIRCLE ( 'NONE', #7469, 12.50000000000000178 ) ;
#7634 = DIRECTION ( 'NONE',  ( -0.9942380540931650135, 0.000000000000000000, -0.1071946444232960011 ) ) ;
#7635 = CARTESIAN_POINT ( 'NONE',  ( -13.08165157527891331, -6.879863062859000955, -437.9641712690918780 ) ) ;
#7636 = DIRECTION ( 'NONE',  ( 0.000000000000000000, -1.000000000000000000, 0.000000000000000000 ) ) ;
#7637 = CARTESIAN_POINT ( 'NONE',  ( -16.21588929933999523, 5.798404451932999137, 190.0071920248299477 ) ) ;
#7638 = LINE ( 'NONE', #1028, #804 ) ;
#7639 =( BOUNDED_SURFACE ( )  B_SPLINE_SURFACE ( 3, 3, ( 
 ( #5399, #6873, #8521, #5343, #3691, #1165, #4444, #8677, #2182, #7723, #6106, #5451, #4545, #9442, #9393, #7820, #466, #2028, #9543, #8729, #2885, #3739, #5295, #6206, #523, #8568, #1213, #4490, #7672, #7768, #411, #4397, #7028, #10350, #2988, #6978, #10249, #7875, #10300, #314, #4601 ),
 ( #3794, #2936, #9492, #2132, #7082, #3590, #6309, #7927, #2236, #10451, #5615, #10565, #1540, #2452, #7343, #3256, #7182, #785, #1597, #8897, #3092, #734, #8783, #3901, #7990, #3851, #572, #5560, #10614, #6535, #7291, #7130, #3037, #2399, #6368, #5503, #6425, #8951, #8090, #9812, #1371 ),
 ( #4065, #6481, #4820, #4010, #3207, #9760, #5667, #1427, #4655, #4713, #9708, #4869, #10398, #4765, #8148, #8035, #9648, #628, #9595, #2290, #8845, #1487, #5720, #683, #3955, #7235, #10505, #3148, #2349, #1645, #6693, #4971, #10025, #835, #3308, #9972, #8298, #9870, #9061, #2613, #5019 ),
 ( #5875, #2670, #9167, #7552, #7499, #4920, #1808, #8246, #5939, #4118, #6586, #5074, #941, #2507, #1698, #8354, #4225, #884, #5771, #992, #9227, #4280, #196, #141, #3527, #3472, #1859, #2718, #7396, #6754, #4170, #5128, #3416, #7445, #6805, #31, #8407, #1046, #4330, #10077, #7603 ) ),
 .UNSPECIFIED., .F., .F., .T. ) 
 B_SPLINE_SURFACE_WITH_KNOTS ( ( 4, 4 ),
 ( 4, 1, 1, 1, 1, 1, 1, 1, 1, 1, 1, 1, 1, 1, 1, 1, 1, 1, 1, 1, 1, 1, 1, 1, 1, 1, 1, 1, 1, 1, 1, 1, 1, 1, 1, 1, 1, 1, 4 ),
 ( 0.000000000000000000, 1.000000000000000000 ),
 ( -0.008481365240538999567, 0.000000000000000000, 0.03418499052141999589, 0.06705543243986999968, 0.09609225505224000541, 0.1212689627326999919, 0.1445858237144000136, 0.1683350686350000014, 0.1924153997444999764, 0.2163475385441999965, 0.2400901845063000140, 0.2638872993326000227, 0.2883641926465000394, 0.3138739111173999841, 0.3400736664824999811, 0.3669224033080000225, 0.3952263667259999780, 0.4258975072560999831, 0.4597904367344000098, 0.4962938553987999990, 0.5331571951194999937, 0.5680640359449000698, 0.5998794348263000176, 0.6292819723868000592, 0.6571102200006999627, 0.6841458463841999516, 0.7104758728877998974, 0.7357936615436999617, 0.7602320418247999756, 0.7841586104491999887, 0.8079717864086000123, 0.8319769714029000562, 0.8557114603086999338, 0.8789861807339000022, 0.9040973669459999584, 0.9330567862467999962, 0.9658526712421000582, 1.000000000000000000, 1.007721702948999987 ),
 .UNSPECIFIED. ) 
 GEOMETRIC_REPRESENTATION_ITEM ( )  RATIONAL_B_SPLINE_SURFACE ( (
 ( 1.236577362560999926, 1.236577362560999926, 1.236577362560999926, 1.236577362560999926, 1.236577362560999926, 1.236577362560999926, 1.236577362560999926, 1.236577362560999926, 1.236577362560999926, 1.236577362560999926, 1.236577362560999926, 1.236577362560999926, 1.236577362560999926, 1.236577362560999926, 1.236577362560999926, 1.236577362560999926, 1.236577362560999926, 1.236577362560999926, 1.236577362560999926, 1.236577362560999926, 1.236577362560999926, 1.236577362560999926, 1.236577362560999926, 1.236577362560999926, 1.236577362560999926, 1.236577362560999926, 1.236577362560999926, 1.236577362560999926, 1.236577362560999926, 1.236577362560999926, 1.236577362560999926, 1.236577362560999926, 1.236577362560999926, 1.236577362560999926, 1.236577362560999926, 1.236577362560999926, 1.236577362560999926, 1.236577362560999926, 1.236577362560999926, 1.236577362560999926, 1.236577362560999926),
 ( 0.9211408791463999712, 0.9211408791463999712, 0.9211408791463999712, 0.9211408791463999712, 0.9211408791463999712, 0.9211408791463999712, 0.9211408791463999712, 0.9211408791463999712, 0.9211408791463999712, 0.9211408791463999712, 0.9211408791463999712, 0.9211408791463999712, 0.9211408791463999712, 0.9211408791463999712, 0.9211408791463999712, 0.9211408791463999712, 0.9211408791463999712, 0.9211408791463999712, 0.9211408791463999712, 0.9211408791463999712, 0.9211408791463999712, 0.9211408791463999712, 0.9211408791463999712, 0.9211408791463999712, 0.9211408791463999712, 0.9211408791463999712, 0.9211408791463999712, 0.9211408791463999712, 0.9211408791463999712, 0.9211408791463999712, 0.9211408791463999712, 0.9211408791463999712, 0.9211408791463999712, 0.9211408791463999712, 0.9211408791463999712, 0.9211408791463999712, 0.9211408791463999712, 0.9211408791463999712, 0.9211408791463999712, 0.9211408791463999712, 0.9211408791463999712),
 ( 0.9211408791463999712, 0.9211408791463999712, 0.9211408791463999712, 0.9211408791463999712, 0.9211408791463999712, 0.9211408791463999712, 0.9211408791463999712, 0.9211408791463999712, 0.9211408791463999712, 0.9211408791463999712, 0.9211408791463999712, 0.9211408791463999712, 0.9211408791463999712, 0.9211408791463999712, 0.9211408791463999712, 0.9211408791463999712, 0.9211408791463999712, 0.9211408791463999712, 0.9211408791463999712, 0.9211408791463999712, 0.9211408791463999712, 0.9211408791463999712, 0.9211408791463999712, 0.9211408791463999712, 0.9211408791463999712, 0.9211408791463999712, 0.9211408791463999712, 0.9211408791463999712, 0.9211408791463999712, 0.9211408791463999712, 0.9211408791463999712, 0.9211408791463999712, 0.9211408791463999712, 0.9211408791463999712, 0.9211408791463999712, 0.9211408791463999712, 0.9211408791463999712, 0.9211408791463999712, 0.9211408791463999712, 0.9211408791463999712, 0.9211408791463999712),
 ( 1.236577362560999926, 1.236577362560999926, 1.236577362560999926, 1.236577362560999926, 1.236577362560999926, 1.236577362560999926, 1.236577362560999926, 1.236577362560999926, 1.236577362560999926, 1.236577362560999926, 1.236577362560999926, 1.236577362560999926, 1.236577362560999926, 1.236577362560999926, 1.236577362560999926, 1.236577362560999926, 1.236577362560999926, 1.236577362560999926, 1.236577362560999926, 1.236577362560999926, 1.236577362560999926, 1.236577362560999926, 1.236577362560999926, 1.236577362560999926, 1.236577362560999926, 1.236577362560999926, 1.236577362560999926, 1.236577362560999926, 1.236577362560999926, 1.236577362560999926, 1.236577362560999926, 1.236577362560999926, 1.236577362560999926, 1.236577362560999926, 1.236577362560999926, 1.236577362560999926, 1.236577362560999926, 1.236577362560999926, 1.236577362560999926, 1.236577362560999926, 1.236577362560999926) ) ) 
 REPRESENTATION_ITEM ( '' )  SURFACE ( )  );
#7640 = CARTESIAN_POINT ( 'NONE',  ( 19.00000000000000000, 0.000000000000000000, 319.9999999999899956 ) ) ;
#7641 = EDGE_CURVE ( 'NONE', #1301, #3871, #9781, .T. ) ;
#7642 = CARTESIAN_POINT ( 'NONE',  ( -1.612612246911211633, -7.337280841968000011, -435.2751398942043579 ) ) ;
#7643 =( REPRESENTATION_RELATIONSHIP ('NONE','NONE', #8468, #4085 ) REPRESENTATION_RELATIONSHIP_WITH_TRANSFORMATION ( #2585 )SHAPE_REPRESENTATION_RELATIONSHIP( ) );
#7644 = DIRECTION ( 'NONE',  ( 0.000000000000000000, 1.000000000000000000, 0.000000000000000000 ) ) ;
#7645 = ORIENTED_EDGE ( 'NONE', *, *, #5793, .F. ) ;
#7646 = CARTESIAN_POINT ( 'NONE',  ( 17.30539973653000629, 4.527429531397997309, 319.9928079742500131 ) ) ;
#7647 = CARTESIAN_POINT ( 'NONE',  ( 10.59678593799237944, -10.61334907845371411, -316.5000000000004547 ) ) ;
#7648 = EDGE_LOOP ( 'NONE', ( #5669, #4401, #1365 ) ) ;
#7649 = FACE_OUTER_BOUND ( 'NONE', #1647, .T. ) ;
#7650 = VERTEX_POINT ( 'NONE', #8393 ) ;
#7651 = CARTESIAN_POINT ( 'NONE',  ( -7.796607451809997258, 10.36222334076000529, -317.4928077629770087 ) ) ;
#7652 = COLOUR_RGB ( '', 0.66274510, 0.83137255, 0.94901961) ;
#7653 = ADVANCED_FACE ( 'NONE', ( #3562 ), #1951, .T. ) ;
#7654 = CARTESIAN_POINT ( 'NONE',  ( 17.80394872498997927, -5.851108818846995518, -317.0792622552969533 ) ) ;
#7655 = EDGE_CURVE ( 'NONE', #4786, #6747, #10288, .T. ) ;
#7656 = CARTESIAN_POINT ( 'NONE',  ( -17.36938240862999905, 0.02134527931159000205, -314.6383426456000052 ) ) ;
#7657 = CIRCLE ( 'NONE', #6517, 3.499999999999998668 ) ;
#7658 = DIRECTION ( 'NONE',  ( 0.000000000000000000, -1.000000000000000000, 0.000000000000000000 ) ) ;
#7659 = CARTESIAN_POINT ( 'NONE',  ( -5.453091809460914874, -9.512452523087866041, 314.4999455543127169 ) ) ;
#7660 = ORIENTED_EDGE ( 'NONE', *, *, #1694, .T. ) ;
#7661 = FILL_AREA_STYLE ('',( #2770 ) ) ;
#7662 = PLANE ( 'NONE',  #3175 ) ;
#7663 = ORIENTED_EDGE ( 'NONE', *, *, #5112, .T. ) ;
#7664 = CARTESIAN_POINT ( 'NONE',  ( -13.93226991011998450, -8.970845217077998868, 191.1197171614399792 ) ) ;
#7665 = ORIENTED_EDGE ( 'NONE', *, *, #9880, .T. ) ;
#7666 = LINE ( 'NONE', #8613, #581 ) ;
#7667 = CARTESIAN_POINT ( 'NONE',  ( -46.74071243416547361, -7.500000000000000000, -414.3237589990478114 ) ) ;
#7668 = EDGE_CURVE ( 'NONE', #4635, #7069, #5974, .T. ) ;
#7669 = CARTESIAN_POINT ( 'NONE',  ( -3.136708848033998187, 12.44064353863999983, 190.4207385301700128 ) ) ;
#7670 = CARTESIAN_POINT ( 'NONE',  ( -0.7282841184975303861, -7.501884272294999434, -434.1436991062553261 ) ) ;
#7671 =( NAMED_UNIT ( * ) SI_UNIT ( $, .STERADIAN. ) SOLID_ANGLE_UNIT ( ) );
#7672 = CARTESIAN_POINT ( 'NONE',  ( -11.26120837094999594, 9.120087085473000954, -302.5071922382879279 ) ) ;
#7673 = CARTESIAN_POINT ( 'NONE',  ( 20.06808111288002294, 0.4071096865243998830, 319.5792614743400009 ) ) ;
#7674 = CARTESIAN_POINT ( 'NONE',  ( -10.23467948400018912, 10.00000000050611959, 189.9999999999997442 ) ) ;
#7675 = CARTESIAN_POINT ( 'NONE',  ( -14.28417481768999941, 5.042936695466000430, 315.0848619657999734 ) ) ;
#7676 = VERTEX_POINT ( 'NONE', #6679 ) ;
#7677 = CARTESIAN_POINT ( 'NONE',  ( 18.44574565965998758, -2.441956922350000614, 190.0071920248299477 ) ) ;
#7678 = ORIENTED_EDGE ( 'NONE', *, *, #9552, .T. ) ;
#7679 = CARTESIAN_POINT ( 'NONE',  ( 12.24957049234000728, 9.976523051824997879, 319.5792614743400009 ) ) ;
#7680 = FACE_OUTER_BOUND ( 'NONE', #4047, .T. ) ;
#7681 = VECTOR ( 'NONE', #10384, 1000.000000000000000 ) ;
#7682 = CARTESIAN_POINT ( 'NONE',  ( -4.462202093987085227, 9.163742891420229242, 315.0000000000000000 ) ) ;
#7683 = CARTESIAN_POINT ( 'NONE',  ( 15.00000000000325961, 7.547804830080786473E-15, -284.9999999999999432 ) ) ;
#7684 = LINE ( 'NONE', #6067, #4712 ) ;
#7685 =( NAMED_UNIT ( * ) SI_UNIT ( $, .STERADIAN. ) SOLID_ANGLE_UNIT ( ) );
#7686 = LINE ( 'NONE', #5210, #8957 ) ;
#7687 = CARTESIAN_POINT ( 'NONE',  ( 7.551447009212327366, -9.031194112208083880, 314.4999434017202589 ) ) ;
#7688 = CARTESIAN_POINT ( 'NONE',  ( -16.77317840633001467, 5.196478383294000025, 190.0071920248299477 ) ) ;
#7689 = AXIS2_PLACEMENT_3D ( 'NONE', #7831, #10208, #10151 ) ;
#7690 = DIRECTION ( 'NONE',  ( 0.9942380540931650135, 0.000000000000000000, 0.1071946444232960011 ) ) ;
#7691 = B_SPLINE_SURFACE_WITH_KNOTS ( 'NONE', 3, 3, ( 
 ( #7725, #10095, #7770, #5297 ),
 ( #2030, #317, #9444, #10302 ),
 ( #3642, #6002, #5346, #3693 ),
 ( #2840, #8622, #5401, #6925 ),
 ( #4548, #413, #6108, #9395 ),
 ( #9345, #8570, #3592, #7822 ),
 ( #5199, #5249, #7877, #6980 ),
 ( #10251, #469, #2887, #6156 ),
 ( #9297, #2081, #1268, #7030 ),
 ( #2938, #8472, #4399, #1928 ),
 ( #9494, #8679, #8954, #686 ),
 ( #8848, #10568, #9653, #7932 ),
 ( #7295, #737, #631, #10352 ),
 ( #3958, #3210, #6484, #2239 ),
 ( #1543, #5670, #6371, #9545 ),
 ( #1374, #4768, #2402, #3905 ),
 ( #8093, #7238, #5507, #9763 ),
 ( #9598, #2185, #1600, #4873 ),
 ( #10454, #7185, #10508, #3095 ),
 ( #8151, #2294, #7993, #3797 ),
 ( #7086, #2990, #8038, #5618 ),
 ( #1430, #5563, #10401, #4659 ),
 ( #3153, #9711, #6266, #1490 ),
 ( #6428, #5454, #8732, #575 ),
 ( #3854, #2352, #7133, #3041 ),
 ( #4716, #8787, #8900, #6312 ),
 ( #4823, #4013, #9171, #3311 ),
 ( #9119, #7398, #1811, #3259 ),
 ( #9922, #4228, #4924, #2616 ),
 ( #2455, #9013, #6538, #4068 ),
 ( #9815, #5942, #4121, #2510 ),
 ( #5827, #7555, #6646, #8200 ),
 ( #4283, #8357, #8249, #7346 ),
 ( #8302, #200, #3475, #9873 ) ),
 .UNSPECIFIED., .F., .F., .F.,
 ( 4, 1, 1, 1, 1, 1, 1, 1, 1, 1, 1, 1, 1, 1, 1, 1, 1, 1, 1, 1, 1, 1, 1, 1, 1, 1, 1, 1, 1, 1, 1, 4 ),
 ( 4, 4 ),
 ( -0.01402646298304000005, 0.000000000000000000, 0.03448275862069000164, 0.06896551724138000328, 0.1034482758621000087, 0.1379310344828000023, 0.1724137931033999926, 0.2068965517240999863, 0.2413793103448000077, 0.2758620689655000291, 0.3103448275861999672, 0.3448275862069000164, 0.3793103448276000100, 0.4137931034483000037, 0.4482758620689999973, 0.4827586206897000465, 0.5172413793103000090, 0.5517241379310000582, 0.5862068965516999963, 0.6206896551723999345, 0.6551724137930999836, 0.6896551724138000328, 0.7241379310344999709, 0.7586206896552000201, 0.7931034482758999582, 0.8275862068966000074, 0.8620689655171999144, 0.8965517241379000746, 0.9310344827586000127, 0.9655172413793000619, 1.000000000000000000, 1.015741306098000063 ),
 ( -0.1697239316932999953, 1.169834029081999960 ),
 .UNSPECIFIED. ) ;
#7692 = DIRECTION ( 'NONE',  ( -0.000000000000000000, 1.000000000000000000, 0.000000000000000000 ) ) ;
#7693 = CARTESIAN_POINT ( 'NONE',  ( 7.974011974874644082, -5.700385244905218585, -525.7480461867619397 ) ) ;
#7694 = CARTESIAN_POINT ( 'NONE',  ( 8.377603294184089222, -8.255708763986199017, 315.0000000000000000 ) ) ;
#7695 = DIRECTION ( 'NONE',  ( -0.9627071798692586890, -0.1321637200910267818, -0.2360670178569624911 ) ) ;
#7696 = ORIENTED_EDGE ( 'NONE', *, *, #3710, .F. ) ;
#7697 = CARTESIAN_POINT ( 'NONE',  ( 4.753602499919002078, 11.02326831536999840, 319.9928079742500131 ) ) ;
#7698 = CARTESIAN_POINT ( 'NONE',  ( -11.66810544104021474, -10.16551412172561442, -316.5000000000004547 ) ) ;
#7699 = LINE ( 'NONE', #2916, #731 ) ;
#7700 = ORIENTED_EDGE ( 'NONE', *, *, #3149, .F. ) ;
#7701 = CARTESIAN_POINT ( 'NONE',  ( 3.239095488904002007, 11.22417384501999038, -317.4928077629770087 ) ) ;
#7702 = EDGE_CURVE ( 'NONE', #1396, #4012, #284, .T. ) ;
#7703 = CARTESIAN_POINT ( 'NONE',  ( 0.2332652941727002271, -12.09631257874000099, -317.5770954168139610 ) ) ;
#7704 = CARTESIAN_POINT ( 'NONE',  ( -17.21448334449999962, 1.351716521078000222, -314.6383426456000052 ) ) ;
#7705 = EDGE_CURVE ( 'NONE', #9387, #10404, #4290, .T. ) ;
#7706 = CARTESIAN_POINT ( 'NONE',  ( -34.37192209818999800, 2.500000000000000000, -461.0868123482000556 ) ) ;
#7707 = VERTEX_POINT ( 'NONE', #6844 ) ;
#7708 = LINE ( 'NONE', #1049, #7803 ) ;
#7709 = EDGE_CURVE ( 'NONE', #4512, #1864, #7488, .T. ) ;
#7710 = CIRCLE ( 'NONE', #9275, 14.00000000000000888 ) ;
#7711 = AXIS2_PLACEMENT_3D ( 'NONE', #2488, #7636, #5914 ) ;
#7712 = CARTESIAN_POINT ( 'NONE',  ( -13.15646768860626636, -9.424872508248350655, 319.0000000000003979 ) ) ;
#7713 = ORIENTED_EDGE ( 'NONE', *, *, #9542, .T. ) ;
#7714 = CARTESIAN_POINT ( 'NONE',  ( -17.74479464825531849, 5.801447790587961784, -316.5000000000004547 ) ) ;
#7715 = ORIENTED_EDGE ( 'NONE', *, *, #9566, .T. ) ;
#7716 = CARTESIAN_POINT ( 'NONE',  ( -10.23467949917770525, -9.999999999493892844, -302.5000000000002842 ) ) ;
#7717 = CARTESIAN_POINT ( 'NONE',  ( -18.90059280977999734, -0.3165218993500001909, -302.5071922382879279 ) ) ;
#7718 = CARTESIAN_POINT ( 'NONE',  ( -5.399293614865643853, -7.500000000000000000, -410.3335483908228980 ) ) ;
#7719 = VECTOR ( 'NONE', #10351, 1000.000000000000000 ) ;
#7720 = CARTESIAN_POINT ( 'NONE',  ( -0.5335076011871895396, -7.487113625182997723, -434.0440531843738086 ) ) ;
#7721 =( BOUNDED_SURFACE ( )  B_SPLINE_SURFACE ( 3, 3, ( 
 ( #4236, #4884, #799, #1441, #8969, #6277, #9722, #4729, #3106, #2362, #2196, #5465, #1386, #4670, #10465, #7945, #5518, #3867, #9610, #10412, #3054, #6322, #8800, #8002, #643, #5628, #3919, #7196, #5576, #8910, #9663, #8858, #1500, #4782, #3968, #7249, #9188, #9242, #7462, #3382, #9130, #9023, #9829, #2685, #2520, #7619, #105, #4346, #8420, #6656 ),
 ( #7513, #1006, #1823, #3489, #9933, #2571, #155, #6709, #1766, #8319, #9986, #4986, #4933, #2467, #5839, #5088, #1873, #5036, #8210, #4294, #954, #4241, #3430, #7566, #5784, #2629, #7408, #210, #1059, #1659, #3323, #3271, #6768, #6549, #5892, #5735, #8369, #50, #848, #4132, #10042, #6603, #5953, #9884, #9076, #5144, #1714, #8262, #901, #4187 ),
 ( #10141, #2783, #9344, #4491, #9443, #412, #1319, #6207, #2133, #6055, #10301, #468, #7769, #1980, #7724, #3692, #8621, #5400, #2733, #6821, #4445, #9493, #6874, #8678, #3591, #10092, #265, #6000, #4398, #5248, #7821, #6979, #4602, #3542, #10196, #10250, #6155, #9295, #8522, #8471, #1925, #2886, #2080, #5197, #365, #3640, #6107, #1116, #7673, #2937 ),
 ( #6924, #315, #1166, #2839, #9394, #2029, #5344, #1267, #4547, #3740, #5296, #8569, #7029, #1214, #3093, #2292, #684, #4821, #2184, #5561, #7183, #8730, #7929, #8846, #3903, #7131, #5452, #1488, #1541, #8036, #6426, #6369, #2400, #4766, #8091, #1598, #2989, #3956, #7236, #7876, #573, #10506, #3151, #9761, #10452, #9709, #5668, #1372, #735, #3852 ) ),
 .UNSPECIFIED., .F., .F., .T. ) 
 B_SPLINE_SURFACE_WITH_KNOTS ( ( 4, 4 ),
 ( 4, 1, 1, 1, 1, 1, 1, 1, 1, 1, 1, 1, 1, 1, 1, 1, 1, 1, 1, 1, 1, 1, 1, 1, 1, 1, 1, 1, 1, 1, 1, 1, 1, 1, 1, 1, 1, 1, 1, 1, 1, 1, 1, 1, 1, 1, 1, 4 ),
 ( 0.000000000000000000, 1.000000000000000000 ),
 ( -0.007735220065637000292, 0.000000000000000000, 0.01939640243318000237, 0.03761844488146999510, 0.05508578791268000513, 0.07214070117811000049, 0.08907871635319999926, 0.1060760411204000053, 0.1230053663521000068, 0.1398981196264000026, 0.1572430803250000064, 0.1753705638249999921, 0.1940981471027000138, 0.2133035938373999962, 0.2331689712455000119, 0.2537734685920000066, 0.2748467046084999699, 0.2963931466709999740, 0.3191313647827999644, 0.3438702858816999886, 0.3714013923646999893, 0.4021771076120999600, 0.4362733060512000161, 0.4736682024355999832, 0.5129970981982000522, 0.5517690204782000896, 0.5879381184936999238, 0.6208232858471999238, 0.6499923806306000529, 0.6755908196375000063, 0.6986884684476999396, 0.7204440523525998952, 0.7419552906557000949, 0.7633235764464999518, 0.7839199576433999450, 0.8036968760389999744, 0.8229339175995999955, 0.8415832447269999683, 0.8594503467308000078, 0.8767353019176999940, 0.8938012255453000598, 0.9107811110342000083, 0.9277285813575999462, 0.9448366096839999617, 0.9623662406040000006, 0.9806256863350999442, 1.000000000000000000, 1.008468161259999940 ),
 .UNSPECIFIED. ) 
 GEOMETRIC_REPRESENTATION_ITEM ( )  RATIONAL_B_SPLINE_SURFACE ( (
 ( 1.236576751392000073, 1.236576751392000073, 1.236576751392000073, 1.236576751392000073, 1.236576751392000073, 1.236576751392000073, 1.236576751392000073, 1.236576751392000073, 1.236576751392000073, 1.236576751392000073, 1.236576751392000073, 1.236576751392000073, 1.236576751392000073, 1.236576751392000073, 1.236576751392000073, 1.236576751392000073, 1.236576751392000073, 1.236576751392000073, 1.236576751392000073, 1.236576751392000073, 1.236576751392000073, 1.236576751392000073, 1.236576751392000073, 1.236576751392000073, 1.236576751392000073, 1.236576751392000073, 1.236576751392000073, 1.236576751392000073, 1.236576751392000073, 1.236576751392000073, 1.236576751392000073, 1.236576751392000073, 1.236576751392000073, 1.236576751392000073, 1.236576751392000073, 1.236576751392000073, 1.236576751392000073, 1.236576751392000073, 1.236576751392000073, 1.236576751392000073, 1.236576751392000073, 1.236576751392000073, 1.236576751392000073, 1.236576751392000073, 1.236576751392000073, 1.236576751392000073, 1.236576751392000073, 1.236576751392000073, 1.236576751392000073, 1.236576751392000073),
 ( 0.9211410828692999653, 0.9211410828692999653, 0.9211410828692999653, 0.9211410828692999653, 0.9211410828692999653, 0.9211410828692999653, 0.9211410828692999653, 0.9211410828692999653, 0.9211410828692999653, 0.9211410828692999653, 0.9211410828692999653, 0.9211410828692999653, 0.9211410828692999653, 0.9211410828692999653, 0.9211410828692999653, 0.9211410828692999653, 0.9211410828692999653, 0.9211410828692999653, 0.9211410828692999653, 0.9211410828692999653, 0.9211410828692999653, 0.9211410828692999653, 0.9211410828692999653, 0.9211410828692999653, 0.9211410828692999653, 0.9211410828692999653, 0.9211410828692999653, 0.9211410828692999653, 0.9211410828692999653, 0.9211410828692999653, 0.9211410828692999653, 0.9211410828692999653, 0.9211410828692999653, 0.9211410828692999653, 0.9211410828692999653, 0.9211410828692999653, 0.9211410828692999653, 0.9211410828692999653, 0.9211410828692999653, 0.9211410828692999653, 0.9211410828692999653, 0.9211410828692999653, 0.9211410828692999653, 0.9211410828692999653, 0.9211410828692999653, 0.9211410828692999653, 0.9211410828692999653, 0.9211410828692999653, 0.9211410828692999653, 0.9211410828692999653),
 ( 0.9211410828692999653, 0.9211410828692999653, 0.9211410828692999653, 0.9211410828692999653, 0.9211410828692999653, 0.9211410828692999653, 0.9211410828692999653, 0.9211410828692999653, 0.9211410828692999653, 0.9211410828692999653, 0.9211410828692999653, 0.9211410828692999653, 0.9211410828692999653, 0.9211410828692999653, 0.9211410828692999653, 0.9211410828692999653, 0.9211410828692999653, 0.9211410828692999653, 0.9211410828692999653, 0.9211410828692999653, 0.9211410828692999653, 0.9211410828692999653, 0.9211410828692999653, 0.9211410828692999653, 0.9211410828692999653, 0.9211410828692999653, 0.9211410828692999653, 0.9211410828692999653, 0.9211410828692999653, 0.9211410828692999653, 0.9211410828692999653, 0.9211410828692999653, 0.9211410828692999653, 0.9211410828692999653, 0.9211410828692999653, 0.9211410828692999653, 0.9211410828692999653, 0.9211410828692999653, 0.9211410828692999653, 0.9211410828692999653, 0.9211410828692999653, 0.9211410828692999653, 0.9211410828692999653, 0.9211410828692999653, 0.9211410828692999653, 0.9211410828692999653, 0.9211410828692999653, 0.9211410828692999653, 0.9211410828692999653, 0.9211410828692999653),
 ( 1.236576751392000073, 1.236576751392000073, 1.236576751392000073, 1.236576751392000073, 1.236576751392000073, 1.236576751392000073, 1.236576751392000073, 1.236576751392000073, 1.236576751392000073, 1.236576751392000073, 1.236576751392000073, 1.236576751392000073, 1.236576751392000073, 1.236576751392000073, 1.236576751392000073, 1.236576751392000073, 1.236576751392000073, 1.236576751392000073, 1.236576751392000073, 1.236576751392000073, 1.236576751392000073, 1.236576751392000073, 1.236576751392000073, 1.236576751392000073, 1.236576751392000073, 1.236576751392000073, 1.236576751392000073, 1.236576751392000073, 1.236576751392000073, 1.236576751392000073, 1.236576751392000073, 1.236576751392000073, 1.236576751392000073, 1.236576751392000073, 1.236576751392000073, 1.236576751392000073, 1.236576751392000073, 1.236576751392000073, 1.236576751392000073, 1.236576751392000073, 1.236576751392000073, 1.236576751392000073, 1.236576751392000073, 1.236576751392000073, 1.236576751392000073, 1.236576751392000073, 1.236576751392000073, 1.236576751392000073, 1.236576751392000073, 1.236576751392000073) ) ) 
 REPRESENTATION_ITEM ( '' )  SURFACE ( )  );
#7722 = ADVANCED_FACE ( 'NONE', ( #3457 ), #5220, .T. ) ;
#7723 = CARTESIAN_POINT ( 'NONE',  ( 14.28705177277001148, 7.417718350405998251, -302.5071922382879279 ) ) ;
#7724 = CARTESIAN_POINT ( 'NONE',  ( -14.08562033053999585, -8.975362299151996126, 319.5792614743400009 ) ) ;
#7725 = CARTESIAN_POINT ( 'NONE',  ( 16.90171868104999930, 0.3834349726278000192, -315.0848619657999734 ) ) ;
#7726 = CARTESIAN_POINT ( 'NONE',  ( -15.10708484062000068, 4.236041382665999500, 315.0848619657999734 ) ) ;
#7727 = ORIENTED_EDGE ( 'NONE', *, *, #10535, .T. ) ;
#7728 = CARTESIAN_POINT ( 'NONE',  ( 8.676965067697993916, -10.10010313590999509, 190.0071920248299477 ) ) ;
#7729 = CARTESIAN_POINT ( 'NONE',  ( -19.98389199037000452, -0.4027620370101000491, 318.8802828394900644 ) ) ;
#7730 = PRESENTATION_LAYER_ASSIGNMENT (  '', '', ( #3090 ) ) ;
#7731 = EDGE_CURVE ( 'NONE', #2333, #6366, #6582, .T. ) ;
#7732 = CARTESIAN_POINT ( 'NONE',  ( -69.81963093799060971, -7.500000000000000000, -370.0675332144908793 ) ) ;
#7733 = CARTESIAN_POINT ( 'NONE',  ( -15.63365740121746406, 3.715179591933191361, 315.0000000000000568 ) ) ;
#7734 = CARTESIAN_POINT ( 'NONE',  ( 20.00000000000000000, 0.000000000000000000, 319.0000000000000000 ) ) ;
#7735 = DIRECTION ( 'NONE',  ( -1.000000000000000000, 0.000000000000000000, 0.000000000000000000 ) ) ;
#7736 = DIRECTION ( 'NONE',  ( 0.000000000000000000, 1.000000000000000000, 0.000000000000000000 ) ) ;
#7737 = CARTESIAN_POINT ( 'NONE',  ( 10.23467949917769282, 9.999999999493891067, -302.4999999999996589 ) ) ;
#7738 = LINE ( 'NONE', #3608, #9265 ) ;
#7739 = CARTESIAN_POINT ( 'NONE',  ( -10.73820067419999980, 9.344548074503993718, 190.0071920248299477 ) ) ;
#7740 = FACE_BOUND ( 'NONE', #3131, .T. ) ;
#7741 = CARTESIAN_POINT ( 'NONE',  ( 19.00000000000000000, 0.000000000000000000, -317.4999999998989892 ) ) ;
#7742 = CARTESIAN_POINT ( 'NONE',  ( -0.4166032843586319201, -7.500000000000000000, -434.8523737515589573 ) ) ;
#7743 = EDGE_CURVE ( 'NONE', #9136, #5334, #7377, .T. ) ;
#7744 = CARTESIAN_POINT ( 'NONE',  ( 6.369677570987301252, -8.818560138237836910, 315.0000000000000000 ) ) ;
#7745 = CARTESIAN_POINT ( 'NONE',  ( 8.587332113753999963, 8.603326289371000968, -314.6383426456000052 ) ) ;
#7746 = VERTEX_POINT ( 'NONE', #8442 ) ;
#7747 = CARTESIAN_POINT ( 'NONE',  ( 16.24851264371998738, 5.765366273007000331, 319.9928079742500131 ) ) ;
#7748 = CARTESIAN_POINT ( 'NONE',  ( -6.468659092863069837, -11.84071280232868872, -316.5000000000004547 ) ) ;
#7749 = CARTESIAN_POINT ( 'NONE',  ( -2.907097610887497741, -12.50000000000000000, -345.9038247371837542 ) ) ;
#7750 = ORIENTED_EDGE ( 'NONE', *, *, #226, .F. ) ;
#7751 = FACE_OUTER_BOUND ( 'NONE', #7913, .T. ) ;
#7752 = CARTESIAN_POINT ( 'NONE',  ( -13.93268562690000678, -9.073621533052005361, -317.0792622552969533 ) ) ;
#7753 = CIRCLE ( 'NONE', #9987, 3.499999999999998668 ) ;
#7754 = DIRECTION ( 'NONE',  ( 0.000000000000000000, 1.000000000000000000, 0.000000000000000000 ) ) ;
#7755 = CARTESIAN_POINT ( 'NONE',  ( 15.84843729815535873, 4.154783985720849948, -314.5664249374441965 ) ) ;
#7756 = ORIENTED_EDGE ( 'NONE', *, *, #507, .F. ) ;
#7757 = CARTESIAN_POINT ( 'NONE',  ( -16.27511603407000251, -5.909078865696000271, 190.0000000000000000 ) ) ;
#7758 = CARTESIAN_POINT ( 'NONE',  ( -10.19008647966648695, -10.76511244458322381, 319.0000000000003979 ) ) ;
#7759 = ORIENTED_EDGE ( 'NONE', *, *, #5820, .F. ) ;
#7760 = CARTESIAN_POINT ( 'NONE',  ( -2.648868200020001229, -12.40196232477001459, 191.1197171614399792 ) ) ;
#7761 = ORIENTED_EDGE ( 'NONE', *, *, #5279, .T. ) ;
#7762 = FACE_OUTER_BOUND ( 'NONE', #8510, .T. ) ;
#7763 = CARTESIAN_POINT ( 'NONE',  ( -5.068019528653000982, -10.96907295785000080, -302.5071922382879279 ) ) ;
#7764 = DIRECTION ( 'NONE',  ( 0.000000000000000000, -1.000000000000000000, 0.000000000000000000 ) ) ;
#7765 = AXIS2_PLACEMENT_3D ( 'NONE', #3002, #8687, #8579 ) ;
#7766 = CARTESIAN_POINT ( 'NONE',  ( -0.6682209595297889937, -7.460089650475999257, -434.3860247085133324 ) ) ;
#7767 = PRESENTATION_STYLE_ASSIGNMENT (( #9293 ) ) ;
#7768 = CARTESIAN_POINT ( 'NONE',  ( -12.33880146245001619, 8.595632119114995362, -302.5071922382879279 ) ) ;
#7769 = CARTESIAN_POINT ( 'NONE',  ( -15.70899585331000559, -7.847162746392004173, 319.5792614743400009 ) ) ;
#7770 = CARTESIAN_POINT ( 'NONE',  ( 17.34693632642999717, 0.4167404706239999923, -314.6383426456000052 ) ) ;
#7771 = CARTESIAN_POINT ( 'NONE',  ( -4.001463906138999604, 9.408458373209999337, 314.8616023057000461 ) ) ;
#7772 = VERTEX_POINT ( 'NONE', #5862 ) ;
#7773 = CARTESIAN_POINT ( 'NONE',  ( -8.506801009283002202, -10.15345907998999486, 190.0071920248299477 ) ) ;
#7774 = CARTESIAN_POINT ( 'NONE',  ( -15.55726960039999973, 7.859060843841005450, 318.8802828394900644 ) ) ;
#7775 = CARTESIAN_POINT ( 'NONE',  ( -53.50011725782000127, 2.500000000000000000, -412.5186446566000313 ) ) ;
#7776 = EDGE_CURVE ( 'NONE', #4332, #289, #338, .T. ) ;
#7777 = AXIS2_PLACEMENT_3D ( 'NONE', #2022, #2775, #4392 ) ;
#7778 = VERTEX_POINT ( 'NONE', #7537 ) ;
#7779 = LINE ( 'NONE', #2894, #3052 ) ;
#7780 = CARTESIAN_POINT ( 'NONE',  ( 18.99997784094000153, 0.3131176371119000490, 319.9999999999899956 ) ) ;
#7781 = CARTESIAN_POINT ( 'NONE',  ( -11.28781796570999951, -4.951468039558000633, 315.0000000000001705 ) ) ;
#7782 = CARTESIAN_POINT ( 'NONE',  ( -13.67659370612792102, -5.618803873927792125, -315.0000000000000000 ) ) ;
#7783 = CARTESIAN_POINT ( 'NONE',  ( -13.09107633769369095, -9.000000000000001776, -400.6378407017721202 ) ) ;
#7784 = DIRECTION ( 'NONE',  ( 0.000000000000000000, 1.000000000000000000, -0.000000000000000000 ) ) ;
#7785 = VECTOR ( 'NONE', #3933, 1000.000000000000114 ) ;
#7786 = CARTESIAN_POINT ( 'NONE',  ( 20.00000000000000000, 7.322330471414334241, -303.5000000000000000 ) ) ;
#7787 = EDGE_CURVE ( 'NONE', #8305, #22, #9680, .T. ) ;
#7788 = CARTESIAN_POINT ( 'NONE',  ( -7.042363285622345259, 8.656086706473072212, -315.0000000000000000 ) ) ;
#7789 = CARTESIAN_POINT ( 'NONE',  ( 17.50000000000000000, 0.000000000000000000, -314.4999343908002629 ) ) ;
#7790 = EDGE_CURVE ( 'NONE', #1052, #1373, #9033, .T. ) ;
#7791 = VECTOR ( 'NONE', #3870, 1000.000000000000000 ) ;
#7792 = ORIENTED_EDGE ( 'NONE', *, *, #4899, .T. ) ;
#7793 = CARTESIAN_POINT ( 'NONE',  ( -18.99987372849000167, -0.5562009942293000275, -317.4999999998989892 ) ) ;
#7794 = DIRECTION ( 'NONE',  ( -0.000000000000000000, 1.000000000000000000, 0.000000000000000000 ) ) ;
#7795 = DIRECTION ( 'NONE',  ( 1.000000000000000000, 0.000000000000000000, 0.000000000000000000 ) ) ;
#7796 = CARTESIAN_POINT ( 'NONE',  ( 2.158263635479988896, -9.422507356620213770, 315.0000000000001137 ) ) ;
#7797 = CARTESIAN_POINT ( 'NONE',  ( 6.322301096779000318, 8.991223814764000011, -314.8616023057000461 ) ) ;
#7798 = CARTESIAN_POINT ( 'NONE',  ( -17.33381025012248600, -7.500000000000000000, -445.8348527500487535 ) ) ;
#7799 = CARTESIAN_POINT ( 'NONE',  ( -79.31727611502927289, -7.500000000000000000, -351.2304352734219606 ) ) ;
#7800 = CARTESIAN_POINT ( 'NONE',  ( -13.22841710535096027, -3.249999999997000177, -437.9939891937848984 ) ) ;
#7801 = ORIENTED_EDGE ( 'NONE', *, *, #3927, .F. ) ;
#7802 = CIRCLE ( 'NONE', #1456, 0.5000000000000172085 ) ;
#7803 = VECTOR ( 'NONE', #10181, 1000.000000000000000 ) ;
#7804 = CARTESIAN_POINT ( 'NONE',  ( 15.21494798568001627, 6.716444321683999519, -317.4928077629770087 ) ) ;
#7805 = CARTESIAN_POINT ( 'NONE',  ( -3.312898553962003056, -11.91959439673999199, -317.5770954168139610 ) ) ;
#7806 = ADVANCED_FACE ( 'NONE', ( #657 ), #5694, .T. ) ;
#7807 = CARTESIAN_POINT ( 'NONE',  ( 8.037373804805000077, -9.179324345868998591, -315.0000000000000000 ) ) ;
#7808 = DIRECTION ( 'NONE',  ( 0.000000000000000000, 0.000000000000000000, 1.000000000000000000 ) ) ;
#7809 = EDGE_LOOP ( 'NONE', ( #1382, #6143, #398, #7608 ) ) ;
#7810 = CARTESIAN_POINT ( 'NONE',  ( -13.37693598625000213, -8.145668871592000926, 190.0000000000000000 ) ) ;
#7811 = LINE ( 'NONE', #2018, #7119 ) ;
#7812 = VERTEX_POINT ( 'NONE', #606 ) ;
#7813 = CARTESIAN_POINT ( 'NONE',  ( -18.56670159326492708, 4.707099758006330958, -316.5000000000004547 ) ) ;
#7814 = EDGE_LOOP ( 'NONE', ( #7379, #3501, #1957, #2032 ) ) ;
#7815 = CARTESIAN_POINT ( 'NONE',  ( -16.91975252613927694, -1.077737682115705642, 314.9999999999999432 ) ) ;
#7816 = CARTESIAN_POINT ( 'NONE',  ( 12.33880146245001619, -8.595632119114995362, -302.5071922382879279 ) ) ;
#7817 = LINE ( 'NONE', #7718, #5571 ) ;
#7818 = PRODUCT_DEFINITION_FORMATION_WITH_SPECIFIED_SOURCE ( 'ANY', '', #2183, .NOT_KNOWN. ) ;
#7819 = DIRECTION ( 'NONE',  ( 5.231090560719999733E-11, 3.356127988687999994E-12, 1.000000000000000000 ) ) ;
#7820 = CARTESIAN_POINT ( 'NONE',  ( 7.736889024074004695, 10.37866566675000435, -302.5071922382879279 ) ) ;
#7821 = CARTESIAN_POINT ( 'NONE',  ( 8.796035389134001292, -11.31703133948999707, 319.5792614743400009 ) ) ;
#7822 = CARTESIAN_POINT ( 'NONE',  ( 17.18263598829999950, -2.199757124398999952, -314.4150829855000211 ) ) ;
#7823 = CARTESIAN_POINT ( 'NONE',  ( -11.96281778373999849, 6.662668310474999522, 315.0848619657999734 ) ) ;
#7824 = ORIENTED_EDGE ( 'NONE', *, *, #7776, .F. ) ;
#7825 = CARTESIAN_POINT ( 'NONE',  ( -5.416173751597343156, -7.500000000000000888, -337.7825848737071510 ) ) ;
#7826 = ORIENTED_EDGE ( 'NONE', *, *, #963, .T. ) ;
#7827 = LINE ( 'NONE', #8576, #9007 ) ;
#7828 = DIRECTION ( 'NONE',  ( 0.000000000000000000, -1.000000000000000000, 0.000000000000000000 ) ) ;
#7829 = CIRCLE ( 'NONE', #9222, 0.5000000000000004441 ) ;
#7830 = EDGE_CURVE ( 'NONE', #8136, #1418, #9623, .T. ) ;
#7831 = CARTESIAN_POINT ( 'NONE',  ( -91.84750071659622961, -2.500000000000000000, -370.2190357451694922 ) ) ;
#7832 = DIRECTION ( 'NONE',  ( 0.000000000000000000, -1.000000000000000000, 0.000000000000000000 ) ) ;
#7833 = CARTESIAN_POINT ( 'NONE',  ( -13.92506561308973545, 5.424300063451886089, 315.0000000000000568 ) ) ;
#7834 = CARTESIAN_POINT ( 'NONE',  ( -11.28781796570999951, -4.951468039558000633, -284.9999999999999432 ) ) ;
#7835 = CARTESIAN_POINT ( 'NONE',  ( -15.63394123731325003, -3.714777356940329511, -315.0000000000000000 ) ) ;
#7836 = CARTESIAN_POINT ( 'NONE',  ( -3.783028835520242161, -2.977152670199212370, -436.1501852806630950 ) ) ;
#7837 = EDGE_CURVE ( 'NONE', #1738, #5739, #2479, .T. ) ;
#7838 = FACE_OUTER_BOUND ( 'NONE', #10015, .T. ) ;
#7839 = CARTESIAN_POINT ( 'NONE',  ( -17.50000000000000000, 0.000000000000000000, -302.5000000000000000 ) ) ;
#7840 = EDGE_CURVE ( 'NONE', #4467, #1953, #4775, .T. ) ;
#7841 = CARTESIAN_POINT ( 'NONE',  ( -2.737251867098380309, 9.374957062059571911, -315.0000000000000000 ) ) ;
#7842 = CARTESIAN_POINT ( 'NONE',  ( -1.232798796115999851, 12.07489154382001040, 189.9229057364800042 ) ) ;
#7843 = CARTESIAN_POINT ( 'NONE',  ( 17.49957620161082872, 0.4465025197079524055, 314.4999504925934275 ) ) ;
#7844 = AXIS2_PLACEMENT_3D ( 'NONE', #8010, #10529, #3174 ) ;
#7845 = ORIENTED_EDGE ( 'NONE', *, *, #8827, .F. ) ;
#7846 = DIRECTION ( 'NONE',  ( 0.4712473909295803454, 0.000000000000000000, -0.8820010751365688906 ) ) ;
#7847 = CARTESIAN_POINT ( 'NONE',  ( -27.98005464532998232, -8.000000000000000000, -417.3300389808354680 ) ) ;
#7848 =( LENGTH_UNIT ( ) NAMED_UNIT ( * ) SI_UNIT ( .MILLI., .METRE. ) );
#7849 = CARTESIAN_POINT ( 'NONE',  ( 16.82367287970800973, -1.353209159721973309, 315.0000000000000000 ) ) ;
#7850 = CARTESIAN_POINT ( 'NONE',  ( -10.49789511286000021, 7.639556387670999982, -314.8616023057000461 ) ) ;
#7851 = EDGE_CURVE ( 'NONE', #1033, #6553, #3081, .T. ) ;
#7852 = CARTESIAN_POINT ( 'NONE',  ( -34.37192209820132405, -7.500000000000000000, -461.0868123482146643 ) ) ;
#7853 = VECTOR ( 'NONE', #3065, 1000.000000000000000 ) ;
#7854 = CARTESIAN_POINT ( 'NONE',  ( 4.863072958135999713, 11.71397411138000422, 320.0770942683900557 ) ) ;
#7855 = CARTESIAN_POINT ( 'NONE',  ( -98.44423576012317767, -2.500000000000000000, -338.7741350709160315 ) ) ;
#7856 = CARTESIAN_POINT ( 'NONE',  ( -0.7870641098475030795, -2.498849777199999789, -434.2253465126299261 ) ) ;
#7857 = VERTEX_POINT ( 'NONE', #274 ) ;
#7858 = CARTESIAN_POINT ( 'NONE',  ( -19.56018822079001040, -0.5268747006259002497, -317.5770954168139610 ) ) ;
#7859 = CARTESIAN_POINT ( 'NONE',  ( 9.398723296113995929, -11.12690316796998324, -317.0792622552969533 ) ) ;
#7860 = DIRECTION ( 'NONE',  ( -0.000000000000000000, 1.000000000000000000, 0.000000000000000000 ) ) ;
#7861 = CARTESIAN_POINT ( 'NONE',  ( 0.000000000000000000, 0.000000000000000000, 315.0000000000000000 ) ) ;
#7862 = ORIENTED_EDGE ( 'NONE', *, *, #7181, .F. ) ;
#7863 = DIRECTION ( 'NONE',  ( 0.000000000000000000, 1.000000000000000000, 0.000000000000000000 ) ) ;
#7864 = CARTESIAN_POINT ( 'NONE',  ( 17.50000000000000711, -8.653813013134384923E-10, -302.5000000000000568 ) ) ;
#7865 = ORIENTED_EDGE ( 'NONE', *, *, #3893, .T. ) ;
#7866 = CARTESIAN_POINT ( 'NONE',  ( 14.83086724907998999, -8.388894394345001615, 191.1197171614399792 ) ) ;
#7867 = ORIENTED_EDGE ( 'NONE', *, *, #1113, .F. ) ;
#7868 = CARTESIAN_POINT ( 'NONE',  ( -51.90260568677000208, -12.50000000000000000, -351.6213581552000278 ) ) ;
#7869 = CARTESIAN_POINT ( 'NONE',  ( -20.10115407781998442, -0.3730669878444000664, -302.9207377450070453 ) ) ;
#7870 = DIRECTION ( 'NONE',  ( 0.9936574763089276452, 0.000000000000000000, 0.1124491875265132140 ) ) ;
#7871 = ORIENTED_EDGE ( 'NONE', *, *, #821, .T. ) ;
#7872 = CARTESIAN_POINT ( 'NONE',  ( -0.8774468747956698511, -7.498360183982002880, -434.2824815778216703 ) ) ;
#7873 = FILL_AREA_STYLE ('',( #522 ) ) ;
#7874 = AXIS2_PLACEMENT_3D ( 'NONE', #8126, #6730, #814 ) ;
#7875 = CARTESIAN_POINT ( 'NONE',  ( -18.78105930652002087, 1.458809753444000767, -302.5071922382879279 ) ) ;
#7876 = CARTESIAN_POINT ( 'NONE',  ( 16.98888588455999127, -6.600739700975996271, 318.8802828394900644 ) ) ;
#7877 = CARTESIAN_POINT ( 'NONE',  ( 16.60805916514000202, -2.908391789136000050, -314.6383426456000052 ) ) ;
#7878 = CARTESIAN_POINT ( 'NONE',  ( -17.18263598829999950, 2.199757124398999952, 314.4150829855000211 ) ) ;
#7879 = EDGE_LOOP ( 'NONE', ( #9526, #8973, #5562, #6196 ) ) ;
#7880 = CARTESIAN_POINT ( 'NONE',  ( -15.60370682163541467, -7.832153051853420145, 190.9999999999995737 ) ) ;
#7881 = CARTESIAN_POINT ( 'NONE',  ( -0.8741371413883790575, -7.485309303923605384, -434.3446856359637991 ) ) ;
#7882 = DIRECTION ( 'NONE',  ( 1.000000000000000000, 0.000000000000000000, 0.000000000000000000 ) ) ;
#7883 = AXIS2_PLACEMENT_3D ( 'NONE', #10063, #1758, #7453 ) ;
#7884 = ORIENTED_EDGE ( 'NONE', *, *, #10174, .T. ) ;
#7885 = FACE_OUTER_BOUND ( 'NONE', #630, .T. ) ;
#7886 = LINE ( 'NONE', #1332, #5355 ) ;
#7887 = AXIS2_PLACEMENT_3D ( 'NONE', #5102, #222, #9201 ) ;
#7888 = CARTESIAN_POINT ( 'NONE',  ( -8.096765587028130540, -8.344222180821057933, -315.0000000000000000 ) ) ;
#7889 = CARTESIAN_POINT ( 'NONE',  ( -7.253510651729878411, -3.465370319632318896, -437.3721018849337270 ) ) ;
#7890 = CARTESIAN_POINT ( 'NONE',  ( 16.99996037728000076, -1.352915776343000118E-09, 314.9999801883000146 ) ) ;
#7891 = CARTESIAN_POINT ( 'NONE',  ( -1.093860234711317325, -8.065417674857998875, -435.9303386687636248 ) ) ;
#7892 = CARTESIAN_POINT ( 'NONE',  ( 9.217250738626690421, 7.977707550455783725, -315.0000000000000568 ) ) ;
#7893 = CARTESIAN_POINT ( 'NONE',  ( 19.56039901294001737, -0.5262506252542004104, 189.9229057364800042 ) ) ;
#7894 = CARTESIAN_POINT ( 'NONE',  ( 12.89405919075535500, 6.798013128617255596, 314.4999472004062682 ) ) ;
#7895 = CIRCLE ( 'NONE', #4303, 2.000000000000001776 ) ;
#7896 = CARTESIAN_POINT ( 'NONE',  ( 16.14934711101999909, -6.043101335943000585, -317.5000000000000000 ) ) ;
#7897 = PRESENTATION_LAYER_ASSIGNMENT (  '', '', ( #4138 ) ) ;
#7898 = CARTESIAN_POINT ( 'NONE',  ( -28.01838671672000203, 2.500000000000000000, -497.7560445212000104 ) ) ;
#7899 = DIRECTION ( 'NONE',  ( 0.8371691043312222691, 2.277112409482203718E-17, 0.5469441386039884945 ) ) ;
#7900 = CARTESIAN_POINT ( 'NONE',  ( 13.89435758465052828, -5.448822883216570823, 315.0000000000000568 ) ) ;
#7901 = CARTESIAN_POINT ( 'NONE',  ( -8.620760283086999820, 8.357092890497000326, -314.8616023057000461 ) ) ;
#7902 = DIRECTION ( 'NONE',  ( 0.9942380540931649024, 0.000000000000000000, 0.1071946444232959872 ) ) ;
#7903 = CARTESIAN_POINT ( 'NONE',  ( 6.386114867952997542, 11.42839325896998481, 320.0770942683900557 ) ) ;
#7904 = CARTESIAN_POINT ( 'NONE',  ( -14.78950287887041526, -5.511224176445043810, -439.2219991040214495 ) ) ;
#7905 = CARTESIAN_POINT ( 'NONE',  ( -0.3057234697441956195, -2.465012315298997780, -434.2611651091350495 ) ) ;
#7906 = ORIENTED_EDGE ( 'NONE', *, *, #9945, .T. ) ;
#7907 = CARTESIAN_POINT ( 'NONE',  ( -20.06704520635998179, -0.4211730678688000440, -317.0792622552969533 ) ) ;
#7908 = CARTESIAN_POINT ( 'NONE',  ( -7.895350322666780940, -9.000000000000001776, -398.4775300148504016 ) ) ;
#7909 = EDGE_CURVE ( 'NONE', #6619, #9376, #6881, .T. ) ;
#7910 = LINE ( 'NONE', #4474, #5623 ) ;
#7911 = EDGE_CURVE ( 'NONE', #168, #4161, #8406, .T. ) ;
#7912 = CARTESIAN_POINT ( 'NONE',  ( -17.38327407059815854, 1.141731131567298885, -314.5066153449287754 ) ) ;
#7913 = EDGE_LOOP ( 'NONE', ( #736, #3799, #9964, #3596 ) ) ;
#7914 = CARTESIAN_POINT ( 'NONE',  ( -13.46369163363000077, 8.092480683229998917, 190.0000000000000000 ) ) ;
#7915 = DIRECTION ( 'NONE',  ( -0.1247904863035891043, 0.000000000000000000, 0.9921831154218023752 ) ) ;
#7916 = ORIENTED_EDGE ( 'NONE', *, *, #4717, .T. ) ;
#7917 = CYLINDRICAL_SURFACE ( 'NONE', #4846, 12.99999999999997868 ) ;
#7918 = ORIENTED_EDGE ( 'NONE', *, *, #7924, .F. ) ;
#7919 = CARTESIAN_POINT ( 'NONE',  ( -9.142607798242581296, -7.997258514545670494, 315.0000000000000000 ) ) ;
#7920 = CARTESIAN_POINT ( 'NONE',  ( -17.77274276690001287, -5.888218767436999457, -302.9207377450070453 ) ) ;
#7921 = EDGE_CURVE ( 'NONE', #911, #2293, #4809, .T. ) ;
#7922 = DIRECTION ( 'NONE',  ( 0.1247904863035870920, 0.000000000000000000, -0.9921831154218027082 ) ) ;
#7923 = CIRCLE ( 'NONE', #39, 3.500000000000020428 ) ;
#7924 = EDGE_CURVE ( 'NONE', #2607, #9600, #4305, .T. ) ;
#7925 = CARTESIAN_POINT ( 'NONE',  ( -0.8256784875976853622, -7.476520917080001105, -434.9497249379059554 ) ) ;
#7926 = SURFACE_SIDE_STYLE ('',( #5450 ) ) ;
#7927 = CARTESIAN_POINT ( 'NONE',  ( 16.55370135034999990, 6.459991253353003948, -302.4229045757450081 ) ) ;
#7928 = PRODUCT_DEFINITION_SHAPE ( 'NONE', 'NONE',  #10637 ) ;
#7929 = CARTESIAN_POINT ( 'NONE',  ( -4.927840600415999361, -12.12262669806999149, 318.8802828394900644 ) ) ;
#7930 = AXIS2_PLACEMENT_3D ( 'NONE', #7543, #3464, #9109 ) ;
#7931 = ORIENTED_EDGE ( 'NONE', *, *, #184, .F. ) ;
#7932 = CARTESIAN_POINT ( 'NONE',  ( 12.28828818102000042, -7.249309191407999897, -314.4150829855000211 ) ) ;
#7933 = CARTESIAN_POINT ( 'NONE',  ( -28.01838671672410896, -7.500000000000000000, -497.7560445212019999 ) ) ;
#7934 = CIRCLE ( 'NONE', #2277, 3.499999999999998668 ) ;
#7935 = ORIENTED_EDGE ( 'NONE', *, *, #10618, .T. ) ;
#7936 = CARTESIAN_POINT ( 'NONE',  ( 7.675832365144997560, -11.11882312068000189, 189.9229057364800042 ) ) ;
#7937 = CARTESIAN_POINT ( 'NONE',  ( -2.571935587102001985, 12.40832180828999398, 318.8802828394900644 ) ) ;
#7938 = CARTESIAN_POINT ( 'NONE',  ( -14.00000000000000000, 2.500000000000000000, -317.5000000000000000 ) ) ;
#7939 = EDGE_CURVE ( 'NONE', #24, #6915, #8919, .T. ) ;
#7940 = CIRCLE ( 'NONE', #3313, 3.500000000000020428 ) ;
#7941 = ORIENTED_EDGE ( 'NONE', *, *, #554, .T. ) ;
#7942 = CARTESIAN_POINT ( 'NONE',  ( 3.971626792229000280, -9.186906450543000702, 315.0848619657999734 ) ) ;
#7943 = DIRECTION ( 'NONE',  ( 4.270328125766856294E-11, 1.000000000000000000, -3.062867458902624639E-11 ) ) ;
#7944 = CARTESIAN_POINT ( 'NONE',  ( -46.74071243419000155, 2.500000000000000000, -414.3237589990000629 ) ) ;
#7945 = CARTESIAN_POINT ( 'NONE',  ( -12.62060098491999938, -8.441142645117002630, 319.9928079742500131 ) ) ;
#7946 = CARTESIAN_POINT ( 'NONE',  ( -15.43598538069024784, -3.955158390306821925, -314.9999999999999432 ) ) ;
#7947 = CARTESIAN_POINT ( 'NONE',  ( -27.18445350464674348, -7.500000000000000000, -447.5567201875090291 ) ) ;
#7948 = DIRECTION ( 'NONE',  ( 0.7426245373610016465, 0.000000000000000000, -0.6697079934638365817 ) ) ;
#7949 = EDGE_LOOP ( 'NONE', ( #6100, #969 ) ) ;
#7950 = FACE_OUTER_BOUND ( 'NONE', #4837, .T. ) ;
#7951 = CARTESIAN_POINT ( 'NONE',  ( -4.714169693051696974, 9.123832451407691835, -314.9999999999999432 ) ) ;
#7952 = CARTESIAN_POINT ( 'NONE',  ( -19.85617711436999144, 1.942822351932998792, 190.4207385301700128 ) ) ;
#7953 = CARTESIAN_POINT ( 'NONE',  ( 17.05557420670857383, 2.295407582498449006, 314.4999494796126669 ) ) ;
#7954 = EDGE_CURVE ( 'NONE', #6648, #4161, #6167, .T. ) ;
#7955 = DIRECTION ( 'NONE',  ( 0.000000000000000000, -1.000000000000000000, 0.000000000000000000 ) ) ;
#7956 = DIRECTION ( 'NONE',  ( 0.8820010751365675583, 0.000000000000000000, 0.4712473909295827323 ) ) ;
#7957 =( GEOMETRIC_REPRESENTATION_CONTEXT ( 3 ) GLOBAL_UNCERTAINTY_ASSIGNED_CONTEXT ( ( #1082 ) ) GLOBAL_UNIT_ASSIGNED_CONTEXT ( ( #1763, #1552, #4076 ) ) REPRESENTATION_CONTEXT ( 'NONE', 'WORKASPACE' ) );
#7958 = APPLICATION_PROTOCOL_DEFINITION ( 'draft international standard', 'automotive_design', 1998, #303 ) ;
#7959 = CARTESIAN_POINT ( 'NONE',  ( -17.50000000000000000, 0.7437989020623000380, -315.0000000000000000 ) ) ;
#7960 = CARTESIAN_POINT ( 'NONE',  ( -6.537559671572000575, 9.400791339334000796, -314.4150829855000211 ) ) ;
#7961 = CARTESIAN_POINT ( 'NONE',  ( -14.00000000000000000, -2.500000000000000000, -387.5000000000000000 ) ) ;
#7962 = CARTESIAN_POINT ( 'NONE',  ( 10.04423725781999543, 10.37030404916000315, 320.0770942683900557 ) ) ;
#7963 = CARTESIAN_POINT ( 'NONE',  ( -2.000000000000000000, 2.500000000000000000, -409.5000000000000568 ) ) ;
#7964 = AXIS2_PLACEMENT_3D ( 'NONE', #10268, #2905, #4569 ) ;
#7965 = CARTESIAN_POINT ( 'NONE',  ( -1.534682465043628152, -2.530859607614999174, -434.5877046317544909 ) ) ;
#7966 = EDGE_LOOP ( 'NONE', ( #9799, #551 ) ) ;
#7967 = CARTESIAN_POINT ( 'NONE',  ( -11.79032227421999757, 10.19419839316000065, -317.0792622552969533 ) ) ;
#7968 = CARTESIAN_POINT ( 'NONE',  ( -17.71107981743001503, -5.830323931021004213, -316.3802825947000201 ) ) ;
#7969 = AXIS2_PLACEMENT_3D ( 'NONE', #9509, #7784, #9456 ) ;
#7970 = VECTOR ( 'NONE', #1027, 1000.000000000000000 ) ;
#7971 = EDGE_CURVE ( 'NONE', #4605, #5301, #2919, .T. ) ;
#7972 = FACE_BOUND ( 'NONE', #6795, .T. ) ;
#7973 = DIRECTION ( 'NONE',  ( 0.7220286942758216142, 0.000000000000000000, 0.6918631112021741414 ) ) ;
#7974 = VECTOR ( 'NONE', #7006, 1000.000000000000000 ) ;
#7976 = ORIENTED_EDGE ( 'NONE', *, *, #4906, .F. ) ;
#7975 = VECTOR ( 'NONE', #2376, 1000.000000000000000 ) ;
#7977 = EDGE_CURVE ( 'NONE', #4961, #10171, #2694, .T. ) ;
#7978 = CARTESIAN_POINT ( 'NONE',  ( 19.78167965760190583, -1.922413304792618405, 319.0000000000003979 ) ) ;
#7979 = VECTOR ( 'NONE', #7986, 1000.000000000000000 ) ;
#7980 = ORIENTED_EDGE ( 'NONE', *, *, #5420, .F. ) ;
#7981 = CARTESIAN_POINT ( 'NONE',  ( 19.30579288353658640, 3.388955136080751274, -316.5000000000004547 ) ) ;
#7982 = ORIENTED_EDGE ( 'NONE', *, *, #5932, .F. ) ;
#7983 = CARTESIAN_POINT ( 'NONE',  ( -11.80673610560780240, -6.814824988023822527, 315.0000000000000000 ) ) ;
#7984 = CARTESIAN_POINT ( 'NONE',  ( -14.97282077145999679, -8.399840787735001868, -302.9207377450070453 ) ) ;
#7985 = EDGE_CURVE ( 'NONE', #6759, #3758, #8782, .T. ) ;
#7986 = DIRECTION ( 'NONE',  ( -0.4712473909295827323, 0.000000000000000000, 0.8820010751365675583 ) ) ;
#7987 =( BOUNDED_SURFACE ( )  B_SPLINE_SURFACE ( 3, 1, ( 
 ( #10429, #1099 ),
 ( #1860, #4331 ),
 ( #299, #9575 ),
 ( #6236, #6039 ),
 ( #6291, #3069 ),
 ( #3577, #6342 ),
 ( #7604, #9523 ) ),
 .UNSPECIFIED., .F., .F., .F. ) 
 B_SPLINE_SURFACE_WITH_KNOTS ( ( 4, 3, 4 ),
 ( 2, 2 ),
 ( 0.000000000000000000, 0.5000000000000000000, 0.9933926304564668630 ),
 ( 0.000000000000000000, 1.000000000000000000 ),
 .UNSPECIFIED. ) 
 GEOMETRIC_REPRESENTATION_ITEM ( )  RATIONAL_B_SPLINE_SURFACE ( (
 ( 1.000000000000000000, 1.000000000000000000),
 ( 0.8025111867385940068, 0.8025111867385940068),
 ( 0.8025111867385940068, 0.8025111867385940068),
 ( 1.000000000000000000, 1.000000000000000000),
 ( 0.8051209498784578367, 0.8051209498784578367),
 ( 0.8025456740775663844, 0.8025456740775663844),
 ( 0.9922741725973256433, 0.9922741725973256433) ) ) 
 REPRESENTATION_ITEM ( '' )  SURFACE ( )  );
#7988 = PRESENTATION_STYLE_ASSIGNMENT (( #5341 ) ) ;
#7989 =( GEOMETRIC_REPRESENTATION_CONTEXT ( 3 ) GLOBAL_UNCERTAINTY_ASSIGNED_CONTEXT ( ( #6025 ) ) GLOBAL_UNIT_ASSIGNED_CONTEXT ( ( #8367, #1821, #208 ) ) REPRESENTATION_CONTEXT ( 'NONE', 'WORKASPACE' ) );
#7990 = CARTESIAN_POINT ( 'NONE',  ( -6.445113046380004818, 11.41524423681998712, -302.4229045757450081 ) ) ;
#7991 = LINE ( 'NONE', #629, #6523 ) ;
#7992 = EDGE_LOOP ( 'NONE', ( #7360, #133, #4990, #7385 ) ) ;
#7993 = CARTESIAN_POINT ( 'NONE',  ( -6.370857846455999507, -9.209451711050000711, -314.6383426456000052 ) ) ;
#7994 = CARTESIAN_POINT ( 'NONE',  ( -17.56954514911999965, -0.4333932196220999788, 314.4150829855000211 ) ) ;
#7995 = ORIENTED_EDGE ( 'NONE', *, *, #8075, .F. ) ;
#7996 = CARTESIAN_POINT ( 'NONE',  ( 14.59598702685000760, -8.048254220853003460, 189.9229057364800042 ) ) ;
#7997 = CARTESIAN_POINT ( 'NONE',  ( -6.404755722164566123, 11.85477825286778497, 190.9999999999996589 ) ) ;
#7998 = DIRECTION ( 'NONE',  ( -0.8820010751365653379, 0.000000000000000000, -0.4712473909295871732 ) ) ;
#7999 = MECHANICAL_DESIGN_GEOMETRIC_PRESENTATION_REPRESENTATION (  '', ( #2000 ), #4223 ) ;
#8000 = CARTESIAN_POINT ( 'NONE',  ( -17.56330558013000243, -0.6698376231023999150, 314.4150829855000211 ) ) ;
#8001 = CARTESIAN_POINT ( 'NONE',  ( 1.295798468764000066, 11.49282963429000048, 320.0000000000000000 ) ) ;
#8002 = CARTESIAN_POINT ( 'NONE',  ( -3.092734256763002065, -11.24153629139000188, 319.9928079742500131 ) ) ;
#8003 = CARTESIAN_POINT ( 'NONE',  ( 10.00000000000000000, -2.500000000000000000, -317.5000000000000000 ) ) ;
#8004 = CARTESIAN_POINT ( 'NONE',  ( -28.01838671672000203, -2.500000000000000000, -497.7560445212000104 ) ) ;
#8005 = CARTESIAN_POINT ( 'NONE',  ( 13.57573464316000056, 3.225916527208000151, 315.0000000000000000 ) ) ;
#8006 = ORIENTED_EDGE ( 'NONE', *, *, #7014, .F. ) ;
#8007 = CARTESIAN_POINT ( 'NONE',  ( -24.00000000000000000, -2.500000000000000000, -380.4979246178999688 ) ) ;
#8008 = CARTESIAN_POINT ( 'NONE',  ( -13.77732760571000092, 8.580179748050001720, 189.9229057364800042 ) ) ;
#8009 = CARTESIAN_POINT ( 'NONE',  ( -17.50000000000000000, 0.000000000000000000, -302.5000000000000000 ) ) ;
#8010 = CARTESIAN_POINT ( 'NONE',  ( -46.74071243419000155, -2.500000000000000000, -414.3237589990000629 ) ) ;
#8011 = CARTESIAN_POINT ( 'NONE',  ( 11.78107618649762500, 6.828710352419061103, 315.0000000000000000 ) ) ;
#8012 = APPLICATION_PROTOCOL_DEFINITION ( 'draft international standard', 'automotive_design', 1998, #9844 ) ;
#8013 = CARTESIAN_POINT ( 'NONE',  ( 3.427628718044569922, -12.33061748745338626, -303.4999999999996589 ) ) ;
#8014 = CARTESIAN_POINT ( 'NONE',  ( 15.56325459994999960, 4.731967449628999844, -314.4150829855000211 ) ) ;
#8015 = LINE ( 'NONE', #2482, #7785 ) ;
#8016 = CARTESIAN_POINT ( 'NONE',  ( -18.87264390915002110, -0.3453755595577998605, 319.9928079742500131 ) ) ;
#8017 = CARTESIAN_POINT ( 'NONE',  ( -0.9555993562026697807, -2.504535365192000373, -434.3261081466394558 ) ) ;
#8018 = ORIENTED_EDGE ( 'NONE', *, *, #3459, .F. ) ;
#8019 = CARTESIAN_POINT ( 'NONE',  ( -8.115185848843001537, 11.51636271397001465, -317.0792622552969533 ) ) ;
#8020 = CARTESIAN_POINT ( 'NONE',  ( 12.86351645698000645, -9.576920946250998767, -316.3802825947000201 ) ) ;
#8021 = PRODUCT_DEFINITION_SHAPE ( 'NONE', 'NONE',  #10631 ) ;
#8022 = CARTESIAN_POINT ( 'NONE',  ( -9.820740202793000861, -9.834836518498999425, 320.0000000000000000 ) ) ;
#8023 = CARTESIAN_POINT ( 'NONE',  ( -0.6467809861380701131, -2.500001317010999813, -434.1465151195269527 ) ) ;
#8024 = CARTESIAN_POINT ( 'NONE',  ( -34.39269738225353024, -2.500000000000000000, -407.7262955260336525 ) ) ;
#8025 = ORIENTED_EDGE ( 'NONE', *, *, #8760, .F. ) ;
#8026 = CARTESIAN_POINT ( 'NONE',  ( 2.572515036489481766, -12.41549478438273191, 319.0000000000003979 ) ) ;
#8027 = ADVANCED_FACE ( 'NONE', ( #7474 ), #8220, .F. ) ;
#8028 = ORIENTED_EDGE ( 'NONE', *, *, #6713, .T. ) ;
#8029 = CARTESIAN_POINT ( 'NONE',  ( 3.357323174585254755, 12.33819210890098894, -316.5000000000004547 ) ) ;
#8030 = ORIENTED_EDGE ( 'NONE', *, *, #6082, .T. ) ;
#8031 = CARTESIAN_POINT ( 'NONE',  ( -8.717521301463110106, -8.144085127293724469, 314.9999999999999432 ) ) ;
#8032 = CARTESIAN_POINT ( 'NONE',  ( 19.56988197685000230, 0.3940236285954000772, -302.4229045757450081 ) ) ;
#8033 = LINE ( 'NONE', #6529, #6336 ) ;
#8034 = ADVANCED_FACE ( 'NONE', ( #7419 ), #6667, .T. ) ;
#8035 = CARTESIAN_POINT ( 'NONE',  ( 8.052748353536003378, 11.53355103076000532, -302.9207377450070453 ) ) ;
#8036 = CARTESIAN_POINT ( 'NONE',  ( 7.493827757249003518, -11.59400354817999457, 318.8802828394900644 ) ) ;
#8037 = ORIENTED_EDGE ( 'NONE', *, *, #5688, .F. ) ;
#8038 = CARTESIAN_POINT ( 'NONE',  ( -8.587332113753999963, -8.603326289371000968, -314.6383426456000052 ) ) ;
#8039 = LINE ( 'NONE', #6486, #938 ) ;
#8040 = EDGE_LOOP ( 'NONE', ( #4419, #6877, #2641, #9749, #2327, #2296 ) ) ;
#8041 = CARTESIAN_POINT ( 'NONE',  ( 17.30294281340998452, -5.653404495199006341, 189.9229057364800042 ) ) ;
#8042 = CARTESIAN_POINT ( 'NONE',  ( -18.18198898035900157, 5.227591177500496400, 190.9999999999996589 ) ) ;
#8043 = DIRECTION ( 'NONE',  ( 0.000000000000000000, 1.000000000000000000, 0.000000000000000000 ) ) ;
#8044 = EDGE_CURVE ( 'NONE', #7389, #3834, #8565, .T. ) ;
#8045 = CARTESIAN_POINT ( 'NONE',  ( -1.266716818501000041, -9.650794245151999462, 314.8616023057000461 ) ) ;
#8046 = FACE_OUTER_BOUND ( 'NONE', #7166, .T. ) ;
#8047 = ADVANCED_FACE ( 'NONE', ( #3500 ), #167, .F. ) ;
#8048 = DIRECTION ( 'NONE',  ( 0.1071946444232947937, 0.000000000000000000, -0.9942380540931651245 ) ) ;
#8049 = CARTESIAN_POINT ( 'NONE',  ( -12.57072393360216722, -9.500000000000001776, -416.1715661968751192 ) ) ;
#8050 = DIRECTION ( 'NONE',  ( 0.1283609399493171321, -0.9912279006826364425, 0.03147567320362415488 ) ) ;
#8051 = CARTESIAN_POINT ( 'NONE',  ( -14.98500449093754483, -3.491150269972000064, -438.4247239981262396 ) ) ;
#8052 = DIRECTION ( 'NONE',  ( -0.8820010751365675583, 0.000000000000000000, -0.4712473909295827323 ) ) ;
#8053 = VERTEX_POINT ( 'NONE', #10000 ) ;
#8054 = CARTESIAN_POINT ( 'NONE',  ( 15.00000000000000000, 0.000000000000000000, -285.0000000000000000 ) ) ;
#8055 = VECTOR ( 'NONE', #7211, 1000.000000000000000 ) ;
#8056 = CIRCLE ( 'NONE', #512, 4.999999999999985789 ) ;
#8057 = CARTESIAN_POINT ( 'NONE',  ( -19.37206517509000037, 1.821913627144001735, 189.9229057364800042 ) ) ;
#8058 = CARTESIAN_POINT ( 'NONE',  ( -83.90876261087991850, -2.366295999999999733, -346.8809236044617137 ) ) ;
#8059 = ADVANCED_FACE ( 'NONE', ( #4356 ), #10179, .F. ) ;
#8060 = CARTESIAN_POINT ( 'NONE',  ( 18.99999673287999968, -1.191366938436000035E-07, 191.0000000000000000 ) ) ;
#8061 = VECTOR ( 'NONE', #8300, 1000.000000000000000 ) ;
#8062 = CYLINDRICAL_SURFACE ( 'NONE', #9655, 4.000000000000000000 ) ;
#8063 = PRODUCT_CONTEXT ( 'NONE', #4546, 'mechanical' ) ;
#8064 = CARTESIAN_POINT ( 'NONE',  ( 15.96459840556376086, -7.551217265629140307, -303.4999999999996589 ) ) ;
#8065 =( BOUNDED_SURFACE ( )  B_SPLINE_SURFACE ( 3, 3, ( 
 ( #6028, #6084, #6134, #6796, #1141, #445, #4421, #10116, #7646, #5976, #7747, #9320, #3565, #9373, #8446, #9269, #1086, #391, #3720, #2756, #1900, #1954, #7697, #340, #5173, #4373, #2007, #3619, #8501, #10168, #2811, #5272, #8547, #1189, #4468, #3664, #6955, #10229, #3882, #10539, #9627, #9681, #9736, #499, #2268, #4745, #5375, #5429, #8016, #659 ),
 ( #8816, #3182, #10325, #2323, #1350, #3934, #10430, #1298, #548, #3767, #7060, #4632, #3018, #2216, #6402, #6237, #1464, #8655, #7962, #4579, #6456, #7903, #7854, #2967, #7214, #10482, #5534, #4797, #8068, #3825, #7159, #3124, #7266, #609, #9524, #5591, #2163, #6344, #3986, #5484, #8708, #7109, #8874, #1516, #10378, #712, #6292, #3070, #9577, #8763 ),
 ( #1404, #4688, #6828, #4247, #9792, #5898, #9197, #10099, #6880, #7625, #6006, #2379, #3496, #4352, #5642, #1122, #7679, #1879, #10049, #2691, #5959, #271, #217, #5150, #323, #163, #6774, #3548, #8927, #1830, #2739, #5095, #7518, #1772, #4404, #8426, #3437, #8326, #9250, #2430, #1571, #5699, #1066, #9301, #5043, #4848, #960, #8376, #1012, #1932 ),
 ( #4300, #3234, #5203, #8478, #6717, #9993, #10592, #3597, #8124, #760, #4044, #7572, #7321, #6510, #8986, #2635, #5254, #3746, #9499, #10147, #10204, #2138, #5404, #1378, #9449, #2942, #7937, #4450, #3801, #6112, #8683, #4553, #6061, #5302, #8528, #1172, #9400, #7774, #6984, #528, #371, #6215, #3859, #2086, #9351, #579, #2035, #2790, #7729, #1325 ) ),
 .UNSPECIFIED., .F., .F., .F. ) 
 B_SPLINE_SURFACE_WITH_KNOTS ( ( 4, 4 ),
 ( 4, 1, 1, 1, 1, 1, 1, 1, 1, 1, 1, 1, 1, 1, 1, 1, 1, 1, 1, 1, 1, 1, 1, 1, 1, 1, 1, 1, 1, 1, 1, 1, 1, 1, 1, 1, 1, 1, 1, 1, 1, 1, 1, 1, 1, 1, 1, 4 ),
 ( 0.000000000000000000, 1.000000000000000000 ),
 ( -0.007735220065637999493, 0.000000000000000000, 0.01939640243318000237, 0.03761844488146999510, 0.05508578791268000513, 0.07214070117811000049, 0.08907871635319999926, 0.1060760411204000053, 0.1230053663521000068, 0.1398981196264000026, 0.1572430803250000064, 0.1753705638249999921, 0.1940981471027000138, 0.2133035938373999962, 0.2331689712455000119, 0.2537734685920000066, 0.2748467046084999699, 0.2963931466709999740, 0.3191313647827999644, 0.3438702858816999886, 0.3714013923646999893, 0.4021771076120999600, 0.4362733060512000161, 0.4736682024355999832, 0.5129970981982000522, 0.5517690204782000896, 0.5879381184936999238, 0.6208232858471999238, 0.6499923806306000529, 0.6755908196375000063, 0.6986884684476999396, 0.7204440523525998952, 0.7419552906557000949, 0.7633235764464999518, 0.7839199576433999450, 0.8036968760389999744, 0.8229339175995999955, 0.8415832447269999683, 0.8594503467308000078, 0.8767353019176999940, 0.8938012255453000598, 0.9107811110342000083, 0.9277285813575999462, 0.9448366096839999617, 0.9623662406040000006, 0.9806256863350999442, 1.000000000000000000, 1.008468161259999940 ),
 .UNSPECIFIED. ) 
 GEOMETRIC_REPRESENTATION_ITEM ( )  RATIONAL_B_SPLINE_SURFACE ( (
 ( 1.236576751392000073, 1.236576751392000073, 1.236576751392000073, 1.236576751392000073, 1.236576751392000073, 1.236576751392000073, 1.236576751392000073, 1.236576751392000073, 1.236576751392000073, 1.236576751392000073, 1.236576751392000073, 1.236576751392000073, 1.236576751392000073, 1.236576751392000073, 1.236576751392000073, 1.236576751392000073, 1.236576751392000073, 1.236576751392000073, 1.236576751392000073, 1.236576751392000073, 1.236576751392000073, 1.236576751392000073, 1.236576751392000073, 1.236576751392000073, 1.236576751392000073, 1.236576751392000073, 1.236576751392000073, 1.236576751392000073, 1.236576751392000073, 1.236576751392000073, 1.236576751392000073, 1.236576751392000073, 1.236576751392000073, 1.236576751392000073, 1.236576751392000073, 1.236576751392000073, 1.236576751392000073, 1.236576751392000073, 1.236576751392000073, 1.236576751392000073, 1.236576751392000073, 1.236576751392000073, 1.236576751392000073, 1.236576751392000073, 1.236576751392000073, 1.236576751392000073, 1.236576751392000073, 1.236576751392000073, 1.236576751392000073, 1.236576751392000073),
 ( 0.9211410828692999653, 0.9211410828692999653, 0.9211410828692999653, 0.9211410828692999653, 0.9211410828692999653, 0.9211410828692999653, 0.9211410828692999653, 0.9211410828692999653, 0.9211410828692999653, 0.9211410828692999653, 0.9211410828692999653, 0.9211410828692999653, 0.9211410828692999653, 0.9211410828692999653, 0.9211410828692999653, 0.9211410828692999653, 0.9211410828692999653, 0.9211410828692999653, 0.9211410828692999653, 0.9211410828692999653, 0.9211410828692999653, 0.9211410828692999653, 0.9211410828692999653, 0.9211410828692999653, 0.9211410828692999653, 0.9211410828692999653, 0.9211410828692999653, 0.9211410828692999653, 0.9211410828692999653, 0.9211410828692999653, 0.9211410828692999653, 0.9211410828692999653, 0.9211410828692999653, 0.9211410828692999653, 0.9211410828692999653, 0.9211410828692999653, 0.9211410828692999653, 0.9211410828692999653, 0.9211410828692999653, 0.9211410828692999653, 0.9211410828692999653, 0.9211410828692999653, 0.9211410828692999653, 0.9211410828692999653, 0.9211410828692999653, 0.9211410828692999653, 0.9211410828692999653, 0.9211410828692999653, 0.9211410828692999653, 0.9211410828692999653),
 ( 0.9211410828692999653, 0.9211410828692999653, 0.9211410828692999653, 0.9211410828692999653, 0.9211410828692999653, 0.9211410828692999653, 0.9211410828692999653, 0.9211410828692999653, 0.9211410828692999653, 0.9211410828692999653, 0.9211410828692999653, 0.9211410828692999653, 0.9211410828692999653, 0.9211410828692999653, 0.9211410828692999653, 0.9211410828692999653, 0.9211410828692999653, 0.9211410828692999653, 0.9211410828692999653, 0.9211410828692999653, 0.9211410828692999653, 0.9211410828692999653, 0.9211410828692999653, 0.9211410828692999653, 0.9211410828692999653, 0.9211410828692999653, 0.9211410828692999653, 0.9211410828692999653, 0.9211410828692999653, 0.9211410828692999653, 0.9211410828692999653, 0.9211410828692999653, 0.9211410828692999653, 0.9211410828692999653, 0.9211410828692999653, 0.9211410828692999653, 0.9211410828692999653, 0.9211410828692999653, 0.9211410828692999653, 0.9211410828692999653, 0.9211410828692999653, 0.9211410828692999653, 0.9211410828692999653, 0.9211410828692999653, 0.9211410828692999653, 0.9211410828692999653, 0.9211410828692999653, 0.9211410828692999653, 0.9211410828692999653, 0.9211410828692999653),
 ( 1.236576751392000073, 1.236576751392000073, 1.236576751392000073, 1.236576751392000073, 1.236576751392000073, 1.236576751392000073, 1.236576751392000073, 1.236576751392000073, 1.236576751392000073, 1.236576751392000073, 1.236576751392000073, 1.236576751392000073, 1.236576751392000073, 1.236576751392000073, 1.236576751392000073, 1.236576751392000073, 1.236576751392000073, 1.236576751392000073, 1.236576751392000073, 1.236576751392000073, 1.236576751392000073, 1.236576751392000073, 1.236576751392000073, 1.236576751392000073, 1.236576751392000073, 1.236576751392000073, 1.236576751392000073, 1.236576751392000073, 1.236576751392000073, 1.236576751392000073, 1.236576751392000073, 1.236576751392000073, 1.236576751392000073, 1.236576751392000073, 1.236576751392000073, 1.236576751392000073, 1.236576751392000073, 1.236576751392000073, 1.236576751392000073, 1.236576751392000073, 1.236576751392000073, 1.236576751392000073, 1.236576751392000073, 1.236576751392000073, 1.236576751392000073, 1.236576751392000073, 1.236576751392000073, 1.236576751392000073, 1.236576751392000073, 1.236576751392000073) ) ) 
 REPRESENTATION_ITEM ( '' )  SURFACE ( )  );
#8066 = CARTESIAN_POINT ( 'NONE',  ( -16.13341719193999779, -6.058597787994999706, -302.5000000000000000 ) ) ;
#8067 = CARTESIAN_POINT ( 'NONE',  ( 1.279515965483999906E-07, 10.00000000755999885, 190.0000000000000000 ) ) ;
#8068 = CARTESIAN_POINT ( 'NONE',  ( -5.958765323235996725, 11.51784730653000643, 320.0770942683900557 ) ) ;
#8069 = FACE_OUTER_BOUND ( 'NONE', #2526, .T. ) ;
#8070 = CARTESIAN_POINT ( 'NONE',  ( -0.7259853328840938369, -2.547408842041999133, -434.4258892964173242 ) ) ;
#8071 = ORIENTED_EDGE ( 'NONE', *, *, #4165, .T. ) ;
#8072 = CARTESIAN_POINT ( 'NONE',  ( -10.44399617086000021, 10.22112142899999476, -317.5770954168139610 ) ) ;
#8073 = AXIS2_PLACEMENT_3D ( 'NONE', #6957, #10231, #2865 ) ;
#8074 = LINE ( 'NONE', #9741, #9782 ) ;
#8075 = EDGE_CURVE ( 'NONE', #4227, #10390, #326, .T. ) ;
#8076 = CARTESIAN_POINT ( 'NONE',  ( -17.81405818021000087, -3.987619665940000502, 320.0000000000000000 ) ) ;
#8077 = UNCERTAINTY_MEASURE_WITH_UNIT (LENGTH_MEASURE( 1.000000000000000082E-05 ), #5105, 'distance_accuracy_value', 'NONE');
#8078 = CARTESIAN_POINT ( 'NONE',  ( -99.26574312853713877, -7.656480000000000175, -341.4806320030483562 ) ) ;
#8079 = CARTESIAN_POINT ( 'NONE',  ( 16.68824139745838409, -1.819223930145251966, -315.0000000000000000 ) ) ;
#8080 = VERTEX_POINT ( 'NONE', #9453 ) ;
#8081 = CARTESIAN_POINT ( 'NONE',  ( 18.18176685080253563, -5.227975112149438885, 319.0000000000003979 ) ) ;
#8082 = ORIENTED_EDGE ( 'NONE', *, *, #9520, .T. ) ;
#8083 = CARTESIAN_POINT ( 'NONE',  ( 10.46398288055045711, 10.66551579990979803, -316.5000000000004547 ) ) ;
#8084 = ORIENTED_EDGE ( 'NONE', *, *, #8123, .F. ) ;
#8085 = CARTESIAN_POINT ( 'NONE',  ( -15.48936016237493973, -3.890032586757016908, 315.0000000000000000 ) ) ;
#8086 = CARTESIAN_POINT ( 'NONE',  ( -19.46046181435998079, -1.651614223715000884, -302.4229045757450081 ) ) ;
#8087 = CARTESIAN_POINT ( 'NONE',  ( -17.01838671672000203, 2.500000000000000000, -497.7560445212000104 ) ) ;
#8088 = EDGE_CURVE ( 'NONE', #1010, #4592, #6894, .T. ) ;
#8089 = SURFACE_SIDE_STYLE ('',( #1536 ) ) ;
#8090 = CARTESIAN_POINT ( 'NONE',  ( -19.60208457603997090, 0.3236162399036999759, -302.4229045757450081 ) ) ;
#8091 = CARTESIAN_POINT ( 'NONE',  ( 12.95981497614000588, -9.523197563374992569, 318.8802828394900644 ) ) ;
#8092 = ORIENTED_EDGE ( 'NONE', *, *, #5002, .T. ) ;
#8093 = CARTESIAN_POINT ( 'NONE',  ( 1.388768300183999882, -9.421618921053999784, -315.0848619657999734 ) ) ;
#8094 = CARTESIAN_POINT ( 'NONE',  ( -9.379635717049819021, -3.022673432387137815, -437.0255164798005012 ) ) ;
#8095 = VERTEX_POINT ( 'NONE', #1176 ) ;
#8096 = VECTOR ( 'NONE', #8914, 1000.000000000000114 ) ;
#8097 = CARTESIAN_POINT ( 'NONE',  ( 12.90475631688000746, -9.082603241465001531, 189.9229057364800042 ) ) ;
#8098 = CARTESIAN_POINT ( 'NONE',  ( 4.467179684046221233, 12.20122392890712959, 190.9999999999996589 ) ) ;
#8099 = DIRECTION ( 'NONE',  ( 0.000000000000000000, -1.000000000000000000, 0.000000000000000000 ) ) ;
#8100 = AXIS2_PLACEMENT_3D ( 'NONE', #1143, #6799, #2111 ) ;
#8101 = CARTESIAN_POINT ( 'NONE',  ( -17.34089965840999881, -0.6440164457022999889, 314.6383426456000052 ) ) ;
#8102 = CARTESIAN_POINT ( 'NONE',  ( -17.80730577449000052, 3.998365122558999563, 320.0000000000000000 ) ) ;
#8103 = AXIS2_PLACEMENT_3D ( 'NONE', #104, #9241, #3541 ) ;
#8104 = LINE ( 'NONE', #7305, #10460 ) ;
#8105 = CARTESIAN_POINT ( 'NONE',  ( 11.22905947253953762, 10.35317575229729137, 319.0000000000005116 ) ) ;
#8106 = CARTESIAN_POINT ( 'NONE',  ( 10.23467949614886763, -10.00000000050611781, 190.0000000000003979 ) ) ;
#8107 = CARTESIAN_POINT ( 'NONE',  ( 0.000000000000000000, 7.937240849781000307, 315.0000000000000000 ) ) ;
#8108 = VERTEX_POINT ( 'NONE', #376 ) ;
#8109 = FACE_OUTER_BOUND ( 'NONE', #2389, .T. ) ;
#8110 = VERTEX_POINT ( 'NONE', #3808 ) ;
#8111 = EDGE_CURVE ( 'NONE', #1033, #911, #3946, .T. ) ;
#8112 = AXIS2_PLACEMENT_3D ( 'NONE', #7861, #6855, #2015 ) ;
#8113 = VERTEX_POINT ( 'NONE', #6989 ) ;
#8114 = DIRECTION ( 'NONE',  ( 0.9554399839384177806, 0.000000000000000000, 0.2951854283188049544 ) ) ;
#8115 = CARTESIAN_POINT ( 'NONE',  ( -17.33327037445098284, -2.718756893828222469E-08, -314.6666037066913191 ) ) ;
#8116 = SHAPE_DEFINITION_REPRESENTATION ( #10419, #5180 ) ;
#8117 = CARTESIAN_POINT ( 'NONE',  ( -18.54125634398931766, -4.746072667744948070, -303.4999999999996589 ) ) ;
#8118 = CARTESIAN_POINT ( 'NONE',  ( 17.14610219660000112, 0.04370646908745000336, -314.8616023057000461 ) ) ;
#8119 = ADVANCED_FACE ( 'NONE', ( #1226 ), #10247, .T. ) ;
#8120 = B_SPLINE_CURVE_WITH_KNOTS ( 'NONE', 3,
 ( #7124, #4812, #5928, #3298, #5122, #23, #3248, #8348, #9862, #829, #1742, #4273, #3410, #9219, #7335, #8239, #190, #4964, #7440, #6579, #4915, #7493, #1797, #9159, #4108, #10606, #8192, #5012, #5067, #6526, #79, #986, #3359, #9054, #2500, #1852, #6685, #876, #5766 ),
 .UNSPECIFIED., .F., .F.,
 ( 4, 1, 1, 1, 1, 1, 1, 1, 1, 1, 1, 1, 1, 1, 1, 1, 1, 1, 1, 1, 1, 1, 1, 1, 1, 1, 1, 1, 1, 1, 1, 1, 1, 1, 1, 1, 4 ),
 ( 0.000000000000000000, 0.02777777777778000015, 0.05555555555556000030, 0.08333333333333001192, 0.1111111111111000027, 0.1388888888888999973, 0.1666666666667000196, 0.1944444444444000109, 0.2222222222222000054, 0.2500000000000000000, 0.2777777777777999946, 0.3055555555555999891, 0.3333333333333000081, 0.3611111111111000027, 0.3888888888888999973, 0.4166666666666999919, 0.4444444444444000109, 0.4722222222222000054, 0.5000000000000000000, 0.5277777777777999946, 0.5555555555555999891, 0.5833333333333000637, 0.6111111111111000582, 0.6388888888888999418, 0.6666666666667000474, 0.6944444444444000109, 0.7222222222222000054, 0.7500000000000000000, 0.7777777777777999946, 0.8055555555555999891, 0.8333333333333000637, 0.8611111111111000582, 0.8888888888888999418, 0.9166666666667000474, 0.9444444444444000109, 0.9722222222222000054, 1.000000000000000000 ),
 .UNSPECIFIED. ) ;
#8121 = CARTESIAN_POINT ( 'NONE',  ( -34.37192209818999800, 2.500000000000000000, -461.0868123482000556 ) ) ;
#8122 = CARTESIAN_POINT ( 'NONE',  ( -4.742836899564842668, -6.886698231682709448, -436.5235822008777973 ) ) ;
#8123 = EDGE_CURVE ( 'NONE', #2874, #5439, #1126, .T. ) ;
#8124 = CARTESIAN_POINT ( 'NONE',  ( 18.20466326549998470, 5.184475519960003886, 318.8802828394900644 ) ) ;
#8125 = LINE ( 'NONE', #761, #7405 ) ;
#8126 = CARTESIAN_POINT ( 'NONE',  ( -2.000000000003786749, -7.500000000000000888, -409.4999999999758415 ) ) ;
#8127 = VERTEX_POINT ( 'NONE', #2040 ) ;
#8128 = CARTESIAN_POINT ( 'NONE',  ( 10.46141074968000062, 10.65879569097000079, -316.3802825947000201 ) ) ;
#8129 = CARTESIAN_POINT ( 'NONE',  ( 14.96823785528000528, -8.299997444912003530, -316.3802825947000201 ) ) ;
#8130 = AXIS2_PLACEMENT_3D ( 'NONE', #5947, #3534, #2726 ) ;
#8131 = ORIENTED_EDGE ( 'NONE', *, *, #4360, .T. ) ;
#8132 = CARTESIAN_POINT ( 'NONE',  ( -16.17578790646000186, -2.500000000000000000, -433.5685902625999688 ) ) ;
#8133 = CARTESIAN_POINT ( 'NONE',  ( -0.7111276526388954355, -7.454525072244997830, -434.4156653599139304 ) ) ;
#8134 = DIRECTION ( 'NONE',  ( 0.000000000000000000, 1.000000000000000000, 0.000000000000000000 ) ) ;
#8135 = FACE_OUTER_BOUND ( 'NONE', #739, .T. ) ;
#8136 = VERTEX_POINT ( 'NONE', #425 ) ;
#8137 = CARTESIAN_POINT ( 'NONE',  ( -4.928966968695707607, -12.12973353869087845, 319.0000000000003979 ) ) ;
#8138 = TOROIDAL_SURFACE ( 'NONE', #9860, 15.50000000000000000, 0.5000000000000000000 ) ;
#8139 = ORIENTED_EDGE ( 'NONE', *, *, #5745, .T. ) ;
#8140 = CYLINDRICAL_SURFACE ( 'NONE', #1592, 3.500000000000006217 ) ;
#8141 = EDGE_LOOP ( 'NONE', ( #1090, #4811, #3688, #10167 ) ) ;
#8142 = CARTESIAN_POINT ( 'NONE',  ( 19.98289592923002544, 0.4160572288964003440, -303.6197174156509391 ) ) ;
#8143 = CLOSED_SHELL ( 'NONE', ( #6068, #7470, #197, #5023, #8119, #8256, #10022, #6485, #2533, #627, #1148, #5679, #3900, #1080, #9649, #2128, #5325, #5612, #8584, #361, #8896, #6750, #8059, #1470, #5152, #4036 ) ) ;
#8144 = CARTESIAN_POINT ( 'NONE',  ( -2.000000000000000000, -10.50000000000000000, -404.4999999999999432 ) ) ;
#8145 = LINE ( 'NONE', #2397, #3678 ) ;
#8146 = CIRCLE ( 'NONE', #7301, 3.500000000000003109 ) ;
#8147 = AXIS2_PLACEMENT_3D ( 'NONE', #6421, #882, #9706 ) ;
#8148 = CARTESIAN_POINT ( 'NONE',  ( 9.338997116452000924, 11.14661793222000519, -302.9207377450070453 ) ) ;
#8149 = CARTESIAN_POINT ( 'NONE',  ( 19.99999035944999903, -7.277437094418000096E-10, -303.5000000000000000 ) ) ;
#8150 = EDGE_LOOP ( 'NONE', ( #2436, #2501, #1971, #7976 ) ) ;
#8151 = CARTESIAN_POINT ( 'NONE',  ( -6.273744347102000241, -8.772995918477999311, -315.0848619657999734 ) ) ;
#8152 = CARTESIAN_POINT ( 'NONE',  ( -17.12432750374000179, -0.4000877216259000058, 314.8616023057000461 ) ) ;
#8153 = ORIENTED_EDGE ( 'NONE', *, *, #121, .F. ) ;
#8154 = CARTESIAN_POINT ( 'NONE',  ( -14.16528011596000169, -7.496216825914998161, 190.0071920248299477 ) ) ;
#8155 = CARTESIAN_POINT ( 'NONE',  ( 6.109815047729934001, 11.91693857169685167, 190.9999999999996589 ) ) ;
#8156 = CARTESIAN_POINT ( 'NONE',  ( 7.529234060647197246, 8.513083068079142279, -315.0000000000000000 ) ) ;
#8157 = CYLINDRICAL_SURFACE ( 'NONE', #3940, 14.00000000000000355 ) ;
#8158 = TOROIDAL_SURFACE ( 'NONE', #5570, 20.50000000000000000, 0.5000000000000000000 ) ;
#8159 = CARTESIAN_POINT ( 'NONE',  ( -1.276003512426000075, -9.874146089817999794, 314.6383426456000052 ) ) ;
#8160 = PRESENTATION_STYLE_ASSIGNMENT (( #7460 ) ) ;
#8161 = DIRECTION ( 'NONE',  ( 0.000000000000000000, -1.000000000000000000, 0.000000000000000000 ) ) ;
#8162 = DIRECTION ( 'NONE',  ( 0.000000000000000000, -1.000000000000000000, 0.000000000000000000 ) ) ;
#8163 = CARTESIAN_POINT ( 'NONE',  ( 17.04674817168136158, 6.551802883975647696, 319.0000000000005116 ) ) ;
#8164 = CARTESIAN_POINT ( 'NONE',  ( -17.50000000000000711, 8.653861160270983887E-10, -302.4999999999999432 ) ) ;
#8165 = CARTESIAN_POINT ( 'NONE',  ( -7.006889269069000115, 6.844138725329000472, 315.0000000000000000 ) ) ;
#8166 = EDGE_LOOP ( 'NONE', ( #1861, #10347, #3438, #9027 ) ) ;
#8167 = CARTESIAN_POINT ( 'NONE',  ( 17.49999998541728985, 5.867334130787307700, 190.0000000000002274 ) ) ;
#8168 =( GEOMETRIC_REPRESENTATION_CONTEXT ( 3 ) GLOBAL_UNCERTAINTY_ASSIGNED_CONTEXT ( ( #8830 ) ) GLOBAL_UNIT_ASSIGNED_CONTEXT ( ( #10504, #4009, #5018 ) ) REPRESENTATION_CONTEXT ( 'NONE', 'WORKASPACE' ) );
#8169 = ADVANCED_FACE ( 'NONE', ( #3703, #1611, #9557 ), #10518, .F. ) ;
#8170 = DIRECTION ( 'NONE',  ( -0.8820010751365675583, 0.000000000000000000, -0.4712473909295827323 ) ) ;
#8171 = STYLED_ITEM ( 'NONE', ( #991 ), #4429 ) ;
#8172 = ADVANCED_FACE ( 'NONE', ( #697 ), #2415, .T. ) ;
#8173 = CARTESIAN_POINT ( 'NONE',  ( 16.37177374402162400, 2.538919766875962658, 314.9999999999999432 ) ) ;
#8174 = CARTESIAN_POINT ( 'NONE',  ( -8.037373804805000077, 9.179324345868998591, -315.0000000000000000 ) ) ;
#8175 = EDGE_CURVE ( 'NONE', #8575, #1218, #8104, .T. ) ;
#8176 = CARTESIAN_POINT ( 'NONE',  ( -30.87192209819000155, -2.500000000000000000, -461.0868123482000556 ) ) ;
#8177 = CARTESIAN_POINT ( 'NONE',  ( -3.729767414393887481, -7.030426507993915664, -436.1287081606701008 ) ) ;
#8178 = CARTESIAN_POINT ( 'NONE',  ( -14.92545173715291007, -5.838463984847977351, -438.6675860777683056 ) ) ;
#8179 = DIRECTION ( 'NONE',  ( -0.9902680687415800209, 0.000000000000000000, -0.1391731009599965763 ) ) ;
#8180 = CYLINDRICAL_SURFACE ( 'NONE', #8314, 0.9999999999999971134 ) ;
#8181 = CARTESIAN_POINT ( 'NONE',  ( -0.2369326581469002602, 12.59441454048000608, -317.0792622552969533 ) ) ;
#8182 = CARTESIAN_POINT ( 'NONE',  ( -1.582650547086741799, -7.339339277715000165, -435.1382983596024019 ) ) ;
#8183 = AXIS2_PLACEMENT_3D ( 'NONE', #9262, #280, #6020 ) ;
#8184 = CARTESIAN_POINT ( 'NONE',  ( -6.294482982547999761, -10.85527983184999989, 320.0000000000000000 ) ) ;
#8185 = CARTESIAN_POINT ( 'NONE',  ( -0.4974408136799305380, -7.489648966280001652, -434.5175391694793916 ) ) ;
#8186 = UNCERTAINTY_MEASURE_WITH_UNIT (LENGTH_MEASURE( 1.000000000000000082E-05 ), #3680, 'distance_accuracy_value', 'NONE');
#8187 = CARTESIAN_POINT ( 'NONE',  ( -72.90663470102438737, -12.00000000000000000, -371.7168990826883714 ) ) ;
#8188 = CARTESIAN_POINT ( 'NONE',  ( 15.24002748250033967, -4.193218933356376965, -315.0000000000001137 ) ) ;
#8189 = EDGE_LOOP ( 'NONE', ( #394, #2671, #2940, #473, #10559, #2497, #9808, #3695 ) ) ;
#8190 = CARTESIAN_POINT ( 'NONE',  ( 17.38327407059815854, -1.141731131567285340, -314.5066153449286048 ) ) ;
#8191 = VERTEX_POINT ( 'NONE', #8743 ) ;
#8192 = CARTESIAN_POINT ( 'NONE',  ( 10.11497662670000075, 9.727801543432001097, -317.5000000000000000 ) ) ;
#8193 = VERTEX_POINT ( 'NONE', #2304 ) ;
#8194 = CARTESIAN_POINT ( 'NONE',  ( -11.70175841024000185, -10.14170047206000014, -303.6197174156509391 ) ) ;
#8195 = DIRECTION ( 'NONE',  ( -0.9968876850330226080, 0.000000000000000000, 0.07883491250392142546 ) ) ;
#8196 = CARTESIAN_POINT ( 'NONE',  ( -7.006889269069000115, -6.844138725329000472, 315.0000000000000000 ) ) ;
#8197 = CARTESIAN_POINT ( 'NONE',  ( -2.971126855877241013, -7.358725049446134037, -435.1576531919852755 ) ) ;
#8198 = CARTESIAN_POINT ( 'NONE',  ( 1.279516016521960085E-07, 10.00000000000000000, 314.4997059534069308 ) ) ;
#8199 = EDGE_LOOP ( 'NONE', ( #2774, #3027 ) ) ;
#8200 = CARTESIAN_POINT ( 'NONE',  ( -17.59334121105999671, -0.04733121045982999903, -314.4150829855000211 ) ) ;
#8201 = CARTESIAN_POINT ( 'NONE',  ( -1.873948611771682149, -12.50000000000000000, -349.2478646809681777 ) ) ;
#8202 = VERTEX_POINT ( 'NONE', #4078 ) ;
#8203 = CARTESIAN_POINT ( 'NONE',  ( 20.04238130943000940, -0.9501178419093005978, 190.4207385301700128 ) ) ;
#8204 = CIRCLE ( 'NONE', #9069, 3.500000000000005773 ) ;
#8205 = CARTESIAN_POINT ( 'NONE',  ( -12.16184652991773163, 9.933083713569276441, 190.9999999999996589 ) ) ;
#8206 = CARTESIAN_POINT ( 'NONE',  ( 16.99910511164432947, 0.8673928700097557343, -314.9999999999999432 ) ) ;
#8207 = CARTESIAN_POINT ( 'NONE',  ( -39.23786858994942151, -9.500000000000001776, -387.8670522075712483 ) ) ;
#8208 = CARTESIAN_POINT ( 'NONE',  ( 6.438474686349000997, -8.964777275824999947, 314.8616023057000461 ) ) ;
#8209 = FACE_OUTER_BOUND ( 'NONE', #9218, .T. ) ;
#8210 = CARTESIAN_POINT ( 'NONE',  ( -10.04423725781999543, -10.37030404916000315, 320.0770942683900557 ) ) ;
#8211 = FACE_OUTER_BOUND ( 'NONE', #1342, .T. ) ;
#8212 = CARTESIAN_POINT ( 'NONE',  ( -18.56827417761491716, 4.704550062028093116, -303.5000000000000000 ) ) ;
#8213 = CARTESIAN_POINT ( 'NONE',  ( 13.18712987686000027, 5.898505050745000311, 315.0848619657999734 ) ) ;
#8214 = ORIENTED_EDGE ( 'NONE', *, *, #6007, .T. ) ;
#8215 = CARTESIAN_POINT ( 'NONE',  ( -20.00000000435073133, 7.322330466772325686, -316.5000000000000000 ) ) ;
#8216 = VERTEX_POINT ( 'NONE', #6439 ) ;
#8217 = DIRECTION ( 'NONE',  ( -0.9396926207858972147, 0.000000000000000000, -0.3420201433256990775 ) ) ;
#8218 = CARTESIAN_POINT ( 'NONE',  ( 14.00164231856462926, 5.362560482542400919, 315.0000000000000000 ) ) ;
#8219 = CONTEXT_DEPENDENT_SHAPE_REPRESENTATION ( #2208, #9650 ) ;
#8220 = PLANE ( 'NONE',  #4301 ) ;
#8221 = CIRCLE ( 'NONE', #4451, 1.000000000000021982 ) ;
#8222 = CARTESIAN_POINT ( 'NONE',  ( -0.6597201369859407860, -2.500000714168999938, -434.1397697187372273 ) ) ;
#8223 = CARTESIAN_POINT ( 'NONE',  ( -10.00000000000000000, -2.500000000000000000, -272.5000000000000000 ) ) ;
#8224 =( NAMED_UNIT ( * ) PLANE_ANGLE_UNIT ( ) SI_UNIT ( $, .RADIAN. ) );
#8225 = DIRECTION ( 'NONE',  ( -1.000000000000000000, 0.000000000000000000, 0.000000000000000000 ) ) ;
#8226 = CARTESIAN_POINT ( 'NONE',  ( -34.37192209820132405, -2.500000000000000000, -461.0868123482146643 ) ) ;
#8227 = ORIENTED_EDGE ( 'NONE', *, *, #5943, .T. ) ;
#8228 = CARTESIAN_POINT ( 'NONE',  ( -13.93264803488000858, 8.974986968055002734, -316.3802825947000201 ) ) ;
#8229 = PRODUCT_DEFINITION ( 'UNKNOWN', '', #6278, #2600 ) ;
#8230 = AXIS2_PLACEMENT_3D ( 'NONE', #8499, #1791, #6026 ) ;
#8231 = CARTESIAN_POINT ( 'NONE',  ( 16.26474538691000049, -5.919460245093000061, 320.0000000000000000 ) ) ;
#8232 = CARTESIAN_POINT ( 'NONE',  ( -0.2899903387719476311, -7.542418068424997735, -434.1586100945300473 ) ) ;
#8233 = DIRECTION ( 'NONE',  ( -0.000000000000000000, 1.000000000000000000, 0.000000000000000000 ) ) ;
#8234 = CARTESIAN_POINT ( 'NONE',  ( 14.02804746531204394, -5.341076607092832162, -315.0000000000000000 ) ) ;
#8235 = VERTEX_POINT ( 'NONE', #9774 ) ;
#8236 = CIRCLE ( 'NONE', #4982, 10.00000000000000000 ) ;
#8237 = CARTESIAN_POINT ( 'NONE',  ( 17.04726327197864322, -2.225800558269675378, -314.5277276635413841 ) ) ;
#8238 = ORIENTED_EDGE ( 'NONE', *, *, #5800, .F. ) ;
#8239 = CARTESIAN_POINT ( 'NONE',  ( -6.537962633339999385, 10.80030782989000038, -317.5000000000000000 ) ) ;
#8240 = ORIENTED_EDGE ( 'NONE', *, *, #3455, .F. ) ;
#8241 = CARTESIAN_POINT ( 'NONE',  ( -19.98381222165001248, 0.4032365313531999784, -303.6197174156509391 ) ) ;
#8242 = EDGE_CURVE ( 'NONE', #6555, #8266, #2250, .T. ) ;
#8243 = CARTESIAN_POINT ( 'NONE',  ( 18.87178158963000030, 0.3573130366704001526, -317.4928077629770087 ) ) ;
#8244 = CARTESIAN_POINT ( 'NONE',  ( 0.000000000000000000, -7.937240849781000307, 315.0000000000000000 ) ) ;
#8245 = VECTOR ( 'NONE', #6433, 1000.000000000000000 ) ;
#8246 = CARTESIAN_POINT ( 'NONE',  ( 16.84215363705000712, 6.757103037815999969, -303.6197174156509391 ) ) ;
#8247 = DIRECTION ( 'NONE',  ( -0.2951854283187965167, 0.000000000000000000, 0.9554399839384203341 ) ) ;
#8248 = ORIENTED_EDGE ( 'NONE', *, *, #7586, .T. ) ;
#8249 = CARTESIAN_POINT ( 'NONE',  ( -17.35477687787999912, 0.3068793820639000303, -314.6383426456000052 ) ) ;
#8250 = EDGE_CURVE ( 'NONE', #10547, #9268, #9785, .T. ) ;
#8251 = CARTESIAN_POINT ( 'NONE',  ( -80.80421425739181984, -2.500000000000000000, -329.3491872523243842 ) ) ;
#8252 = VERTEX_POINT ( 'NONE', #6382 ) ;
#8253 = CARTESIAN_POINT ( 'NONE',  ( 20.00511239988002998, -0.1020359997562000631, 191.1197171614399792 ) ) ;
#8254 = CARTESIAN_POINT ( 'NONE',  ( -2.000000000003786749, -8.000000000000000000, -409.4999999999758415 ) ) ;
#8255 = CARTESIAN_POINT ( 'NONE',  ( -72.90663470102438737, -12.50000000000000000, -371.7168990826883714 ) ) ;
#8256 = ADVANCED_FACE ( 'NONE', ( #587 ), #7721, .T. ) ;
#8257 = CARTESIAN_POINT ( 'NONE',  ( -7.659536309752155603, -7.500000000000000888, -398.9184288142485570 ) ) ;
#8258 = CARTESIAN_POINT ( 'NONE',  ( -11.16929996816999804, 10.37059603288001419, 191.1197171614399792 ) ) ;
#8259 = MECHANICAL_DESIGN_GEOMETRIC_PRESENTATION_REPRESENTATION (  '', ( #531 ), #6023 ) ;
#8260 = CARTESIAN_POINT ( 'NONE',  ( 12.28828818102000042, -7.249309191407999897, 314.4150829855000211 ) ) ;
#8261 = PLANE ( 'NONE',  #6741 ) ;
#8262 = CARTESIAN_POINT ( 'NONE',  ( 19.59086175841999378, -0.09594170647769000027, 320.0770942683900557 ) ) ;
#8263 = CARTESIAN_POINT ( 'NONE',  ( -19.63511402242740189, -9.000000000000001776, -416.9332195861429113 ) ) ;
#8264 = CARTESIAN_POINT ( 'NONE',  ( -13.93992802816217136, 8.979094264391768832, -303.4999999999990905 ) ) ;
#8265 = CARTESIAN_POINT ( 'NONE',  ( 8.587332113753999963, 8.603326289371000968, 314.6383426456000052 ) ) ;
#8266 = VERTEX_POINT ( 'NONE', #4656 ) ;
#8267 = DIRECTION ( 'NONE',  ( 0.000000000000000000, 0.000000000000000000, -1.000000000000000000 ) ) ;
#8268 = VERTEX_POINT ( 'NONE', #6265 ) ;
#8269 = EDGE_CURVE ( 'NONE', #8127, #10485, #5616, .T. ) ;
#8270 = AXIS2_PLACEMENT_3D ( 'NONE', #7282, #8890, #10558 ) ;
#8271 = DIRECTION ( 'NONE',  ( 1.000000000000000000, 0.000000000000000000, 0.000000000000000000 ) ) ;
#8272 = CARTESIAN_POINT ( 'NONE',  ( -8.377603294184089222, 8.255708763986199017, 315.0000000000000000 ) ) ;
#8273 = ITEM_DEFINED_TRANSFORMATION ( 'NONE', 'NONE', #1303,  #2817 ) ;
#8274 = CARTESIAN_POINT ( 'NONE',  ( -7.659536309752155603, -9.000000000000001776, -398.9184288142485570 ) ) ;
#8275 = VERTEX_POINT ( 'NONE', #4011 ) ;
#8276 = CARTESIAN_POINT ( 'NONE',  ( 3.370560865743999823, -11.33032003377000052, -302.5000000000000000 ) ) ;
#8277 = CARTESIAN_POINT ( 'NONE',  ( -8.993684809926110191, -8.000000000000000000, -419.2513267189134467 ) ) ;
#8278 = CARTESIAN_POINT ( 'NONE',  ( -14.96085924495833375, -6.066301387037711379, -438.5231907234968958 ) ) ;
#8279 = CIRCLE ( 'NONE', #8103, 12.50000000000001243 ) ;
#8280 = CYLINDRICAL_SURFACE ( 'NONE', #5492, 4.000000000000008882 ) ;
#8281 = CARTESIAN_POINT ( 'NONE',  ( -37.82921798586438911, -7.500000000000000888, -422.3602549205895684 ) ) ;
#8282 = CARTESIAN_POINT ( 'NONE',  ( 4.976995723842001951, 12.11314212604000318, -316.3802825947000201 ) ) ;
#8283 = CARTESIAN_POINT ( 'NONE',  ( 18.95675155274000190, -0.9190877154199000865, 320.0000000000000000 ) ) ;
#8284 = CARTESIAN_POINT ( 'NONE',  ( -1.076134953867535549, -7.413975726001998723, -434.6066135568960362 ) ) ;
#8285 = CARTESIAN_POINT ( 'NONE',  ( -19.63511402242640713, -8.000000000000000000, -416.9332195861427977 ) ) ;
#8286 = CARTESIAN_POINT ( 'NONE',  ( 13.97602275805729555, -5.383336353019481990, -315.0000000000001137 ) ) ;
#8287 = ORIENTED_EDGE ( 'NONE', *, *, #9172, .T. ) ;
#8288 = CARTESIAN_POINT ( 'NONE',  ( 0.000000000000000000, 10.54711710274999881, -315.0000000000001137 ) ) ;
#8289 = EDGE_LOOP ( 'NONE', ( #2325, #9089, #2336, #7019 ) ) ;
#8290 = DIRECTION ( 'NONE',  ( -0.000000000000000000, 1.000000000000000000, 0.000000000000000000 ) ) ;
#8291 = ORIENTED_EDGE ( 'NONE', *, *, #8864, .T. ) ;
#8292 = CARTESIAN_POINT ( 'NONE',  ( -12.81291305286001858, -9.603378439332990624, -303.6197174156509391 ) ) ;
#8293 = EDGE_CURVE ( 'NONE', #9710, #6471, #2350, .T. ) ;
#8294 = CARTESIAN_POINT ( 'NONE',  ( -6.235150775465998052, -10.74512744517000407, -317.4928077629770087 ) ) ;
#8295 = CARTESIAN_POINT ( 'NONE',  ( -24.05731444175778577, -7.500000000000000000, -497.1993521173619683 ) ) ;
#8296 = FILL_AREA_STYLE_COLOUR ( '', #6633 ) ;
#8297 = EDGE_CURVE ( 'NONE', #10381, #5864, #1369, .T. ) ;
#8298 = CARTESIAN_POINT ( 'NONE',  ( -19.39478698591998551, 3.379789856048000196, -302.9207377450070453 ) ) ;
#8299 = STYLED_ITEM ( 'NONE', ( #1129 ), #8917 ) ;
#8300 = DIRECTION ( 'NONE',  ( -1.705302565823999938E-14, -1.000000000000000000, -0.000000000000000000 ) ) ;
#8301 = VERTEX_POINT ( 'NONE', #10566 ) ;
#8302 = CARTESIAN_POINT ( 'NONE',  ( -16.90189876424999937, 0.3838616842170000099, -315.0848619657999734 ) ) ;
#8303 = ADVANCED_FACE ( 'NONE', ( #5505 ), #3208, .T. ) ;
#8304 = LINE ( 'NONE', #8251, #6088 ) ;
#8305 = VERTEX_POINT ( 'NONE', #3796 ) ;
#8306 = CARTESIAN_POINT ( 'NONE',  ( 19.95847042008000827, -0.9399586737018998939, 191.1197171614399792 ) ) ;
#8307 = CYLINDRICAL_SURFACE ( 'NONE', #8466, 0.5000000000000004441 ) ;
#8308 = CARTESIAN_POINT ( 'NONE',  ( 11.33749276371198889, 7.060967193034009881, -315.0000000000000000 ) ) ;
#8309 = CIRCLE ( 'NONE', #6420, 10.00000000000000533 ) ;
#8310 = DIRECTION ( 'NONE',  ( 0.9627073223221466192, 0.1321616141473069550, 0.2360676159351401404 ) ) ;
#8311 = CARTESIAN_POINT ( 'NONE',  ( -3.128426543399003279, 12.35671765842998582, 191.1197171614399792 ) ) ;
#8312 = CIRCLE ( 'NONE', #3670, 3.500000000000003109 ) ;
#8313 = AXIS2_PLACEMENT_3D ( 'NONE', #3626, #6908, #9970 ) ;
#8314 = AXIS2_PLACEMENT_3D ( 'NONE', #815, #6173, #2099 ) ;
#8315 = CARTESIAN_POINT ( 'NONE',  ( 17.12243801299000268, -0.5826713957640000663, 314.8616023057000461 ) ) ;
#8316 = SURFACE_STYLE_FILL_AREA ( #5837 ) ;
#8317 = EDGE_CURVE ( 'NONE', #6682, #7412, #9544, .T. ) ;
#8318 = DIRECTION ( 'NONE',  ( 0.000000000000000000, 1.000000000000000000, 0.000000000000000000 ) ) ;
#8319 = CARTESIAN_POINT ( 'NONE',  ( -17.33400069613001193, -5.617198899843996784, 320.0770942683900557 ) ) ;
#8320 = DIRECTION ( 'NONE',  ( 0.000000000000000000, -1.000000000000000000, 0.000000000000000000 ) ) ;
#8321 = CARTESIAN_POINT ( 'NONE',  ( 19.99984324442397110, 0.5882482212486084272, -303.5000000000000000 ) ) ;
#8322 = CARTESIAN_POINT ( 'NONE',  ( 17.56970546055000071, -0.4338786413876999926, 314.4150829855000211 ) ) ;
#8323 = ORIENTED_EDGE ( 'NONE', *, *, #8365, .T. ) ;
#8324 = CARTESIAN_POINT ( 'NONE',  ( -12.04241988217490622, -9.990194130379512316, 190.9999999999995737 ) ) ;
#8325 = STYLED_ITEM ( 'NONE', ( #351 ), #5374 ) ;
#8326 = CARTESIAN_POINT ( 'NONE',  ( -15.60880606785999980, 7.925821651060998008, 319.5792614743400009 ) ) ;
#8327 = ORIENTED_EDGE ( 'NONE', *, *, #2082, .T. ) ;
#8328 = CARTESIAN_POINT ( 'NONE',  ( -1.418770314803618815, -2.864400061963000788, -435.1301057596324995 ) ) ;
#8329 = CARTESIAN_POINT ( 'NONE',  ( -10.90962076852776796, 7.272180451173178461, 315.0000000000000000 ) ) ;
#8330 = CARTESIAN_POINT ( 'NONE',  ( -76.73771626751471331, -12.00000000000000000, -359.8175430394059617 ) ) ;
#8331 = VERTEX_POINT ( 'NONE', #2237 ) ;
#8332 = CARTESIAN_POINT ( 'NONE',  ( -1.166138655389787004, -2.532879817436650693, -434.4904125972011570 ) ) ;
#8333 = CARTESIAN_POINT ( 'NONE',  ( -72.90663470096859555, -2.500000000000000000, -371.7168990827444190 ) ) ;
#8334 = CARTESIAN_POINT ( 'NONE',  ( -2.575131942425901599, -6.981554778721000609, -435.4819513718353505 ) ) ;
#8335 = DIRECTION ( 'NONE',  ( 0.000000000000000000, 1.000000000000000000, -0.000000000000000000 ) ) ;
#8336 = CARTESIAN_POINT ( 'NONE',  ( -0.1338654248474115960, -2.334823577025999075, -433.9583966923889875 ) ) ;
#8337 = DIRECTION ( 'NONE',  ( 0.000000000000000000, 0.000000000000000000, -1.000000000000000000 ) ) ;
#8338 = CARTESIAN_POINT ( 'NONE',  ( 20.06802617119998899, -0.4069525832282999134, -317.0792622552969533 ) ) ;
#8339 =( GEOMETRIC_REPRESENTATION_CONTEXT ( 3 ) GLOBAL_UNCERTAINTY_ASSIGNED_CONTEXT ( ( #3994 ) ) GLOBAL_UNIT_ASSIGNED_CONTEXT ( ( #1566, #2210, #5530 ) ) REPRESENTATION_CONTEXT ( 'NONE', 'WORKASPACE' ) );
#8340 = FACE_OUTER_BOUND ( 'NONE', #7348, .T. ) ;
#8341 = FACE_OUTER_BOUND ( 'NONE', #2876, .T. ) ;
#8342 = CARTESIAN_POINT ( 'NONE',  ( 10.00000000000000000, -2.500000000000000000, -315.0000000000000000 ) ) ;
#8343 = CARTESIAN_POINT ( 'NONE',  ( 4.252979419060003430, -9.197563690522738256, -315.0000000000000568 ) ) ;
#8344 = EDGE_LOOP ( 'NONE', ( #7544, #994 ) ) ;
#8345 = CARTESIAN_POINT ( 'NONE',  ( 0.9068124364724619024, -10.00021929074745231, -314.4998859403474967 ) ) ;
#8346 = DIRECTION ( 'NONE',  ( -0.8820010751365675583, 0.000000000000000000, -0.4712473909295827323 ) ) ;
#8347 = EDGE_LOOP ( 'NONE', ( #6098, #6783, #8828, #2446 ) ) ;
#8348 = CARTESIAN_POINT ( 'NONE',  ( -15.28484891664999878, 6.814525346632999359, -317.5000000000000000 ) ) ;
#8349 = ORIENTED_EDGE ( 'NONE', *, *, #9425, .T. ) ;
#8350 = CARTESIAN_POINT ( 'NONE',  ( -19.97256092624000701, 0.5562539513971997973, -303.6197174156509391 ) ) ;
#8351 = CARTESIAN_POINT ( 'NONE',  ( 11.58474654271000048, -9.740515853135002899, -317.5770954168139610 ) ) ;
#8352 = CARTESIAN_POINT ( 'NONE',  ( -16.89986669904000394, 0.5583209492923999484, -315.0848619657999734 ) ) ;
#8353 = CARTESIAN_POINT ( 'NONE',  ( 0.000000000000000000, 0.000000000000000000, 0.000000000000000000 ) ) ;
#8354 = CARTESIAN_POINT ( 'NONE',  ( 8.030503796230000546, 11.45221762926000153, -303.6197174156509391 ) ) ;
#8355 = DIRECTION ( 'NONE',  ( 0.000000000000000000, 1.000000000000000000, -0.000000000000000000 ) ) ;
#8356 = ORIENTED_EDGE ( 'NONE', *, *, #2143, .F. ) ;
#8357 = CARTESIAN_POINT ( 'NONE',  ( -17.13182678275000370, 0.2945984483948000388, -314.8616023057000461 ) ) ;
#8358 = CARTESIAN_POINT ( 'NONE',  ( -1.646600138488000020, 11.47371312023999934, -302.5000000000000000 ) ) ;
#8359 = ORIENTED_EDGE ( 'NONE', *, *, #1195, .F. ) ;
#8360 = CARTESIAN_POINT ( 'NONE',  ( 1.252197968601000744, -12.57265714642999477, 190.4207385301700128 ) ) ;
#8361 = DIRECTION ( 'NONE',  ( 0.000000000000000000, -1.000000000000000000, 0.000000000000000000 ) ) ;
#8362 = FACE_OUTER_BOUND ( 'NONE', #10097, .T. ) ;
#8363 = FACE_OUTER_BOUND ( 'NONE', #9208, .T. ) ;
#8364 = CARTESIAN_POINT ( 'NONE',  ( -7.802724030307999215, 11.60041405728999919, 190.4207385301700128 ) ) ;
#8365 = EDGE_CURVE ( 'NONE', #8559, #6686, #5823, .T. ) ;
#8366 = CARTESIAN_POINT ( 'NONE',  ( 6.388932193737000276, -8.746770244069999478, 315.0848619657999734 ) ) ;
#8367 =( LENGTH_UNIT ( ) NAMED_UNIT ( * ) SI_UNIT ( .MILLI., .METRE. ) );
#8368 = DIRECTION ( 'NONE',  ( -0.000000000000000000, 1.000000000000000000, 0.000000000000000000 ) ) ;
#8369 = CARTESIAN_POINT ( 'NONE',  ( 14.51666864684999680, -8.103202762918000346, 320.0770942683900557 ) ) ;
#8370 = VECTOR ( 'NONE', #8217, 1000.000000000000227 ) ;
#8371 = CARTESIAN_POINT ( 'NONE',  ( 5.118368704603114087E-10, 10.00000000003099210, 314.4999681336588537 ) ) ;
#8372 = CARTESIAN_POINT ( 'NONE',  ( -9.254661647337840691, 11.09380704494734537, -303.4999999999990905 ) ) ;
#8373 = CARTESIAN_POINT ( 'NONE',  ( 17.20518503178000103, 1.389427005613000032, 314.6383426456000052 ) ) ;
#8374 = ORIENTED_EDGE ( 'NONE', *, *, #88, .T. ) ;
#8375 = CARTESIAN_POINT ( 'NONE',  ( -50.43337757792475173, -2.500000000000000000, -464.9351226150769207 ) ) ;
#8376 = CARTESIAN_POINT ( 'NONE',  ( -20.08948270067001829, 0.1023867585008999687, 319.5792614743400009 ) ) ;
#8377 = EDGE_CURVE ( 'NONE', #5498, #78, #7991, .T. ) ;
#8378 = EDGE_CURVE ( 'NONE', #4540, #4067, #10615, .T. ) ;
#8379 = CARTESIAN_POINT ( 'NONE',  ( -8.042176964449417653, -2.829147761587998744, -436.6151782268157717 ) ) ;
#8380 = CARTESIAN_POINT ( 'NONE',  ( -4.532266548732788003, 9.152838354191798587, 315.0000000000000568 ) ) ;
#8381 = ITEM_DEFINED_TRANSFORMATION ( 'NONE', 'NONE', #1135,  #2817 ) ;
#8382 = DIRECTION ( 'NONE',  ( 0.6697079934638360266, -2.513318893526203994E-16, 0.7426245373610022016 ) ) ;
#8383 = EDGE_LOOP ( 'NONE', ( #985, #593 ) ) ;
#8384 = CARTESIAN_POINT ( 'NONE',  ( 12.36246450207000080, -8.718211867489999989, -302.5000000000000000 ) ) ;
#8385 = CARTESIAN_POINT ( 'NONE',  ( -5.273242226636224217, -7.500000000000000000, -350.0814130718403590 ) ) ;
#8386 = EDGE_CURVE ( 'NONE', #9889, #3371, #3257, .T. ) ;
#8387 = FACE_OUTER_BOUND ( 'NONE', #1680, .T. ) ;
#8388 = FACE_OUTER_BOUND ( 'NONE', #5469, .T. ) ;
#8389 = DIRECTION ( 'NONE',  ( 0.000000000000000000, 0.000000000000000000, -1.000000000000000000 ) ) ;
#8390 = FACE_BOUND ( 'NONE', #8199, .T. ) ;
#8391 = FACE_OUTER_BOUND ( 'NONE', #5815, .T. ) ;
#8392 = CARTESIAN_POINT ( 'NONE',  ( 8.385892640053510760, -5.754955315852783748, -525.7042111492452250 ) ) ;
#8393 = CARTESIAN_POINT ( 'NONE',  ( -85.25464975288055314, -7.500000000000000000, -378.3143625557585779 ) ) ;
#8394 = CARTESIAN_POINT ( 'NONE',  ( 15.75853520210212366, -3.543431633405212722, -315.0000000000000000 ) ) ;
#8395 = ORIENTED_EDGE ( 'NONE', *, *, #8443, .T. ) ;
#8396 = LINE ( 'NONE', #7798, #9868 ) ;
#8397 = CARTESIAN_POINT ( 'NONE',  ( 19.99999036626000048, 4.642009117057000143E-09, -316.5000000000000000 ) ) ;
#8398 = ORIENTED_EDGE ( 'NONE', *, *, #6967, .F. ) ;
#8399 = LINE ( 'NONE', #7388, #7085 ) ;
#8400 = ORIENTED_EDGE ( 'NONE', *, *, #1881, .T. ) ;
#8401 = DIRECTION ( 'NONE',  ( 0.000000000000000000, -1.000000000000000000, 0.000000000000000000 ) ) ;
#8402 = CARTESIAN_POINT ( 'NONE',  ( 17.42196264042997100, -5.530423875593995398, -317.5770954168139610 ) ) ;
#8403 = EDGE_CURVE ( 'NONE', #3792, #5421, #4456, .T. ) ;
#8404 = CARTESIAN_POINT ( 'NONE',  ( -14.98500449093754483, -6.508849730028000380, -438.4247239981262396 ) ) ;
#8405 = DIRECTION ( 'NONE',  ( 0.000000000000000000, 0.000000000000000000, 1.000000000000000000 ) ) ;
#8406 = CIRCLE ( 'NONE', #4637, 15.00000000000000711 ) ;
#8407 = CARTESIAN_POINT ( 'NONE',  ( -19.31742247159998271, 3.345204157467998929, -303.6197174156509391 ) ) ;
#8408 = CARTESIAN_POINT ( 'NONE',  ( -11.05317446192489328, -7.762181880391725741, 314.4999466939158879 ) ) ;
#8409 = ORIENTED_EDGE ( 'NONE', *, *, #6614, .T. ) ;
#8410 = CARTESIAN_POINT ( 'NONE',  ( 16.27944536538999998, -5.903984566639000064, 190.0000000000000000 ) ) ;
#8411 = CARTESIAN_POINT ( 'NONE',  ( 3.664414252749999878, 11.29532875361999977, -302.5000000000000000 ) ) ;
#8412 = ORIENTED_EDGE ( 'NONE', *, *, #10296, .F. ) ;
#8413 = CARTESIAN_POINT ( 'NONE',  ( -14.84250811591998520, -8.483799448551005540, 190.4207385301700128 ) ) ;
#8414 = CARTESIAN_POINT ( 'NONE',  ( 17.19853431801041665, -2.231396706186351775, -314.4944826805095772 ) ) ;
#8415 = CARTESIAN_POINT ( 'NONE',  ( 10.02545106797884955, 7.672278800222119166, -315.0000000000000000 ) ) ;
#8416 = CARTESIAN_POINT ( 'NONE',  ( 14.84250811591998520, 8.483799448551005540, 190.4207385301700128 ) ) ;
#8417 = AXIS2_PLACEMENT_3D ( 'NONE', #7582, #8577, #1222 ) ;
#8418 = CARTESIAN_POINT ( 'NONE',  ( 10.58688533405000065, -7.844683714540999553, 314.6383426456000052 ) ) ;
#8419 = FACE_OUTER_BOUND ( 'NONE', #509, .T. ) ;
#8420 = CARTESIAN_POINT ( 'NONE',  ( 18.87264390915002110, 0.3453755595577998605, 319.9928079742500131 ) ) ;
#8421 = DIRECTION ( 'NONE',  ( 8.659560562355704463E-17, 0.7071067811864846231, -0.7071067811866105224 ) ) ;
#8422 = CARTESIAN_POINT ( 'NONE',  ( 6.687916194383508817, 11.79215677264877016, -303.4999999999990905 ) ) ;
#8423 = CARTESIAN_POINT ( 'NONE',  ( 17.16710485141000220, 2.239552065056999997, 314.4150829855000211 ) ) ;
#8424 = ORIENTED_EDGE ( 'NONE', *, *, #786, .F. ) ;
#8425 = CARTESIAN_POINT ( 'NONE',  ( -38.59226537204000351, -2.500000000000000000, -500.7880554352000217 ) ) ;
#8426 = CARTESIAN_POINT ( 'NONE',  ( -13.92742316895000165, 9.072312068102004190, 319.5792614743400009 ) ) ;
#8427 = LINE ( 'NONE', #3550, #816 ) ;
#8428 = CARTESIAN_POINT ( 'NONE',  ( -2.737672117484407863, 9.377292971636139285, 315.0000000000000568 ) ) ;
#8429 = DIRECTION ( 'NONE',  ( -0.9712267471052612455, 0.000000000000000000, -0.2381566831044910626 ) ) ;
#8430 = ORIENTED_EDGE ( 'NONE', *, *, #7615, .F. ) ;
#8431 = CARTESIAN_POINT ( 'NONE',  ( -3.664414252749999878, -11.29532875361999977, -302.5000000000000000 ) ) ;
#8432 = EDGE_CURVE ( 'NONE', #6682, #2603, #9278, .T. ) ;
#8433 = DIRECTION ( 'NONE',  ( 1.000000000000000000, 0.000000000000000000, 0.000000000000000000 ) ) ;
#8434 = CARTESIAN_POINT ( 'NONE',  ( -6.057194280361955840, -7.279247941943998157, -436.0403555669980733 ) ) ;
#8435 = CARTESIAN_POINT ( 'NONE',  ( -14.44867893690424410, 4.983401360453108886, -315.0000000000000568 ) ) ;
#8437 = CARTESIAN_POINT ( 'NONE',  ( 18.70165185342001735, 1.614428960665998503, 190.0071920248299477 ) ) ;
#8436 = VECTOR ( 'NONE', #1065, 1000.000000000000000 ) ;
#8438 = LINE ( 'NONE', #4365, #6287 ) ;
#8439 = DIRECTION ( 'NONE',  ( 0.5945784143118931775, 0.000000000000000000, 0.8040376292402952041 ) ) ;
#8440 = CARTESIAN_POINT ( 'NONE',  ( 9.297655439795304844, -5.886997446105330489, -525.2645627975454090 ) ) ;
#8441 = AXIS2_PLACEMENT_3D ( 'NONE', #10279, #6184, #2759 ) ;
#8442 = CARTESIAN_POINT ( 'NONE',  ( -24.51838671671999847, 2.500000000000000000, -497.7560445212000104 ) ) ;
#8443 = EDGE_CURVE ( 'NONE', #10456, #6576, #885, .T. ) ;
#8444 = AXIS2_PLACEMENT_3D ( 'NONE', #6708, #209, #1713 ) ;
#8445 = VERTEX_POINT ( 'NONE', #1749 ) ;
#8446 = CARTESIAN_POINT ( 'NONE',  ( 13.45825946928999706, 7.955479052880997770, 319.9928079742500131 ) ) ;
#8447 = DIRECTION ( 'NONE',  ( -0.8820010751365675583, 0.000000000000000000, -0.4712473909295827323 ) ) ;
#8448 = ORIENTED_EDGE ( 'NONE', *, *, #2346, .T. ) ;
#8449 = DIRECTION ( 'NONE',  ( 1.000000000000000000, 0.000000000000000000, 0.000000000000000000 ) ) ;
#8450 = ORIENTED_EDGE ( 'NONE', *, *, #5279, .F. ) ;
#8451 = APPLICATION_CONTEXT ( 'automotive_design' ) ;
#8452 = DIRECTION ( 'NONE',  ( 0.000000000000000000, -1.000000000000000000, 0.000000000000000000 ) ) ;
#8453 = CARTESIAN_POINT ( 'NONE',  ( 13.71837527932998491, -8.620941849619004671, -317.5770954168139610 ) ) ;
#8454 = AXIS2_PLACEMENT_3D ( 'NONE', #3944, #7278, #3138 ) ;
#8455 = CARTESIAN_POINT ( 'NONE',  ( -16.28527389671999970, 3.844447514156999812, -314.4150829855000211 ) ) ;
#8456 = CARTESIAN_POINT ( 'NONE',  ( 16.94482484090574204, 2.428629253473844507, -314.5323066871361561 ) ) ;
#8457 = CARTESIAN_POINT ( 'NONE',  ( 10.00000000000000000, -2.500000000000000000, -315.0000000000000000 ) ) ;
#8458 = ORIENTED_EDGE ( 'NONE', *, *, #2933, .F. ) ;
#8459 = CARTESIAN_POINT ( 'NONE',  ( -16.84157450053000105, -5.300668178571999789, 190.0000000000000000 ) ) ;
#8460 = CARTESIAN_POINT ( 'NONE',  ( -16.38421488526942582, -7.181844560322185878, 319.0000000000003979 ) ) ;
#8461 = ORIENTED_EDGE ( 'NONE', *, *, #7591, .F. ) ;
#8462 = DIRECTION ( 'NONE',  ( 0.000000000000000000, -1.000000000000000000, 0.000000000000000000 ) ) ;
#8463 = CARTESIAN_POINT ( 'NONE',  ( -17.50000000000125056, -1.338989683019597976E-14, -314.4944826805095204 ) ) ;
#8464 = CARTESIAN_POINT ( 'NONE',  ( -18.27982664221999443, -2.925785484622998922, -302.5071922382879279 ) ) ;
#8465 = CARTESIAN_POINT ( 'NONE',  ( 20.04745173227997768, 0.9063373766989004654, 190.4207385301700128 ) ) ;
#8466 = AXIS2_PLACEMENT_3D ( 'NONE', #4179, #9286, #8361 ) ;
#8467 = CARTESIAN_POINT ( 'NONE',  ( -0.8419518381993236211, -7.499550864176998566, -434.2611549955821033 ) ) ;
#8468 = SHAPE_REPRESENTATION ( 'MAS-686', ( #7315, #112, #3549, #6104, #9210, #1476, #4912, #7484, #8855, #626, #1303, #10234, #5073, #6975, #1135 ), #8339 ) ;
#8469 = AXIS2_PLACEMENT_3D ( 'NONE', #4918, #3203, #8947 ) ;
#8470 = DIRECTION ( 'NONE',  ( 0.000000000000000000, 1.000000000000000000, -0.000000000000000000 ) ) ;
#8471 = CARTESIAN_POINT ( 'NONE',  ( 17.04863675780999088, -6.660280422001000566, 319.5792614743400009 ) ) ;
#8472 = CARTESIAN_POINT ( 'NONE',  ( 14.43094748301999886, -5.211771040651000497, -314.8616023057000461 ) ) ;
#8473 = CARTESIAN_POINT ( 'NONE',  ( -15.92197846796999983, 3.582977715798000062, 314.8616023057000461 ) ) ;
#8474 = ORIENTED_EDGE ( 'NONE', *, *, #7830, .F. ) ;
#8475 = AXIS2_PLACEMENT_3D ( 'NONE', #6293, #3935, #5430 ) ;
#8476 = CARTESIAN_POINT ( 'NONE',  ( 19.78120799650142203, -1.924098540961039605, 190.9999999999995737 ) ) ;
#8477 = EDGE_LOOP ( 'NONE', ( #6198, #2551, #2819, #2633 ) ) ;
#8478 = CARTESIAN_POINT ( 'NONE',  ( 19.96334758606998605, 0.8982332345458986511, 318.8802828394900644 ) ) ;
#8479 = CIRCLE ( 'NONE', #10205, 3.499999999999999556 ) ;
#8480 = ORIENTED_EDGE ( 'NONE', *, *, #10150, .T. ) ;
#8481 = DIRECTION ( 'NONE',  ( -1.905029615504999997E-09, 1.123812154447000012E-10, 1.000000000000000000 ) ) ;
#8482 = CARTESIAN_POINT ( 'NONE',  ( 8.778709539581399213, 8.123450746681353252, 315.0000000000000000 ) ) ;
#8483 = CARTESIAN_POINT ( 'NONE',  ( -11.71572875295034066, -12.49999999989693755, 190.9999999999999432 ) ) ;
#8484 = AXIS2_PLACEMENT_3D ( 'NONE', #1034, #5223, #241 ) ;
#8485 = CIRCLE ( 'NONE', #10206, 3.499999999999999112 ) ;
#8486 = CARTESIAN_POINT ( 'NONE',  ( -1.582652182125599660, -2.660653890702000091, -435.1382991101020821 ) ) ;
#8487 = FACE_OUTER_BOUND ( 'NONE', #9141, .T. ) ;
#8488 = EDGE_CURVE ( 'NONE', #4386, #1953, #9573, .T. ) ;
#8489 = CARTESIAN_POINT ( 'NONE',  ( -13.35722247976206312, -6.863431602888001137, -438.0342774710397862 ) ) ;
#8490 = DIRECTION ( 'NONE',  ( -1.351443457106230809E-13, -1.000000000000000000, -1.086844694983562447E-13 ) ) ;
#8491 = CARTESIAN_POINT ( 'NONE',  ( -18.12330621507001638, 3.185864752952001222, 190.0071920248299477 ) ) ;
#8492 = PLANE ( 'NONE',  #5423 ) ;
#8493 = DIRECTION ( 'NONE',  ( 0.000000000000000000, 0.000000000000000000, 1.000000000000000000 ) ) ;
#8494 = EDGE_CURVE ( 'NONE', #344, #4674, #6335, .T. ) ;
#8495 = B_SPLINE_CURVE_WITH_KNOTS ( 'NONE', 3,
 ( #1473, #4754, #2440, #5710, #824, #8023, #6574 ),
 .UNSPECIFIED., .F., .F.,
 ( 4, 1, 1, 1, 4 ),
 ( 0.000000000000000000, 0.2500000000000000000, 0.5000000000000000000, 0.7500000000000000000, 1.000000000000000000 ),
 .UNSPECIFIED. ) ;
#8496 = CARTESIAN_POINT ( 'NONE',  ( -1.551408298843238054, -7.347010659421000511, -435.2528021670048020 ) ) ;
#8497 = UNCERTAINTY_MEASURE_WITH_UNIT (LENGTH_MEASURE( 1.000000000000000082E-05 ), #4168, 'distance_accuracy_value', 'NONE');
#8498 = ADVANCED_BREP_SHAPE_REPRESENTATION ( '', ( #8977, #2817 ), #3838 ) ;
#8499 = CARTESIAN_POINT ( 'NONE',  ( -2.000000000000000000, 4.200000000000000178, -409.5000000000000000 ) ) ;
#8500 = ORIENTED_EDGE ( 'NONE', *, *, #7971, .T. ) ;
#8501 = CARTESIAN_POINT ( 'NONE',  ( -5.823281502584001679, 10.83177932830000501, 319.9928079742500131 ) ) ;
#8502 = CARTESIAN_POINT ( 'NONE',  ( -50.43337757792475173, -7.500000000000000000, -464.9351226150769207 ) ) ;
#8503 = FACE_OUTER_BOUND ( 'NONE', #6058, .T. ) ;
#8504 = VERTEX_POINT ( 'NONE', #3417 ) ;
#8505 = CARTESIAN_POINT ( 'NONE',  ( -0.2281161656705998908, 11.39695712172000164, -317.4928077629770087 ) ) ;
#8506 = CARTESIAN_POINT ( 'NONE',  ( 16.01024372474999069, -7.613620273433004293, -317.0792622552969533 ) ) ;
#8507 = EDGE_CURVE ( 'NONE', #932, #5188, #5151, .T. ) ;
#8508 = CARTESIAN_POINT ( 'NONE',  ( -17.34500932694999875, 0.6070218422356999932, -314.6383426456000052 ) ) ;
#8509 = LINE ( 'NONE', #2116, #2457 ) ;
#8510 = EDGE_LOOP ( 'NONE', ( #54, #7237, #9334, #491 ) ) ;
#8511 = CARTESIAN_POINT ( 'NONE',  ( -18.95710617844000012, -0.9155000425601000913, 190.0000000000000000 ) ) ;
#8512 = CARTESIAN_POINT ( 'NONE',  ( -18.71196753105320099, -4.439097376277244322, 319.0000000000003979 ) ) ;
#8513 = ORIENTED_EDGE ( 'NONE', *, *, #10192, .T. ) ;
#8514 = DIRECTION ( 'NONE',  ( -0.8820010751365676693, 0.000000000000000000, -0.4712473909295822883 ) ) ;
#8515 = VERTEX_POINT ( 'NONE', #6755 ) ;
#8516 = DIRECTION ( 'NONE',  ( 0.8820010751365664481, 0.000000000000000000, 0.4712473909295847307 ) ) ;
#8517 = CARTESIAN_POINT ( 'NONE',  ( -71.87348570190857799, -7.500000000000000888, -375.0609390264727949 ) ) ;
#8518 = ADVANCED_FACE ( 'NONE', ( #4171 ), #2453, .T. ) ;
#8519 = CARTESIAN_POINT ( 'NONE',  ( 19.78498824058000594, 1.878712957033002340, 191.1197171614399792 ) ) ;
#8520 = CARTESIAN_POINT ( 'NONE',  ( -0.7493775555037957004, -7.501813285185003011, -434.1959393140418797 ) ) ;
#8521 = CARTESIAN_POINT ( 'NONE',  ( 18.90059280977999734, 0.3165218993500001909, -302.5071922382879279 ) ) ;
#8522 = CARTESIAN_POINT ( 'NONE',  ( 16.36040776911000449, -7.306617842034003552, 319.5792614743400009 ) ) ;
#8523 = DIRECTION ( 'NONE',  ( 0.000000000000000000, 0.000000000000000000, 1.000000000000000000 ) ) ;
#8524 = CARTESIAN_POINT ( 'NONE',  ( -16.80445917461999983, 3.015803745947999825, 314.4150829855000211 ) ) ;
#8525 = ORIENTED_EDGE ( 'NONE', *, *, #5731, .T. ) ;
#8526 = CARTESIAN_POINT ( 'NONE',  ( 10.73820067419999980, -9.344548074503993718, 190.0071920248299477 ) ) ;
#8527 = ORIENTED_EDGE ( 'NONE', *, *, #6940, .T. ) ;
#8528 = CARTESIAN_POINT ( 'NONE',  ( -12.95981497614000588, 9.523197563374992569, 318.8802828394900644 ) ) ;
#8529 = ADVANCED_FACE ( 'NONE', ( #5722 ), #706, .F. ) ;
#8530 = CARTESIAN_POINT ( 'NONE',  ( -16.90887668763000207, 0.2823175147257999673, 315.0848619657999734 ) ) ;
#8531 = VECTOR ( 'NONE', #6987, 1000.000000000000000 ) ;
#8532 = CARTESIAN_POINT ( 'NONE',  ( -16.33370887135086491, 2.613387004688928261, 315.0000000000000568 ) ) ;
#8533 = CARTESIAN_POINT ( 'NONE',  ( -14.79012398733999767, -1.483731117707002278, 315.0000000000001705 ) ) ;
#8534 = CARTESIAN_POINT ( 'NONE',  ( -2.081727251769323050, -2.733745693750686989, -435.4229215395205301 ) ) ;
#8535 = DIRECTION ( 'NONE',  ( 0.000000000000000000, 1.000000000000000000, 0.000000000000000000 ) ) ;
#8536 = CARTESIAN_POINT ( 'NONE',  ( -9.896141615135300995, -5.985941516016800357, -437.8432809189114892 ) ) ;
#8537 = CARTESIAN_POINT ( 'NONE',  ( -16.40967564559107927, 2.462589562615133065, -315.0000000000000000 ) ) ;
#8538 = DIRECTION ( 'NONE',  ( 0.000000000000000000, 1.000000000000000000, 0.000000000000000000 ) ) ;
#8539 = DIRECTION ( 'NONE',  ( -0.000000000000000000, 1.000000000000000000, 0.000000000000000000 ) ) ;
#8540 = B_SPLINE_SURFACE_WITH_KNOTS ( 'NONE', 3, 1, ( 
 ( #2647, #9902 ),
 ( #4207, #8929 ),
 ( #4150, #5754 ),
 ( #6566, #1573 ),
 ( #9041, #1676 ),
 ( #763, #6512 ),
 ( #917, #123 ),
 ( #5702, #8988 ),
 ( #3399, #6673 ),
 ( #2593, #9847 ),
 ( #7428, #6788 ),
 ( #1840, #5459 ),
 ( #10407, #10256 ) ),
 .UNSPECIFIED., .F., .F., .F.,
 ( 4, 1, 1, 1, 1, 1, 1, 1, 1, 1, 4 ),
 ( 2, 2 ),
 ( 0.01923076923076999858, 0.09935897435896999530, 0.1794871794871999993, 0.2596153846154000133, 0.3397435897436000274, 0.5000000000000000000, 0.6602564102564000281, 0.7403846153845999867, 0.8205128205128000562, 0.9006410256410000148, 0.9807692307692000844 ),
 ( 0.000000000000000000, 1.000000000000000000 ),
 .UNSPECIFIED. ) ;
#8541 = CARTESIAN_POINT ( 'NONE',  ( -37.45790571715708239, -9.000000000000001776, -422.6951089172942488 ) ) ;
#8542 = CARTESIAN_POINT ( 'NONE',  ( -0.6600669447125837586, -9.000000000000001776, -421.9279756761403632 ) ) ;
#8543 = CARTESIAN_POINT ( 'NONE',  ( 15.42265167804419512, -3.971230633025111700, 315.0000000000000568 ) ) ;
#8544 = CARTESIAN_POINT ( 'NONE',  ( 3.932702496464000497, 9.868769537474999964, -314.4150829855000211 ) ) ;
#8545 = ORIENTED_EDGE ( 'NONE', *, *, #2002, .T. ) ;
#8546 = PRODUCT_RELATED_PRODUCT_CATEGORY ( 'part', '', ( #8784 ) ) ;
#8547 = CARTESIAN_POINT ( 'NONE',  ( -10.54985698513999637, 9.422913819601998142, 319.9928079742500131 ) ) ;
#8548 = CARTESIAN_POINT ( 'NONE',  ( 8.094664229193856642, -11.44201740537352840, -316.5000000000004547 ) ) ;
#8549 = DIRECTION ( 'NONE',  ( -0.000000000000000000, 1.000000000000000000, 0.000000000000000000 ) ) ;
#8550 = ORIENTED_EDGE ( 'NONE', *, *, #2556, .F. ) ;
#8551 = CARTESIAN_POINT ( 'NONE',  ( -2.000000000003786749, -7.500000000000000888, -409.4999999999758415 ) ) ;
#8552 = CARTESIAN_POINT ( 'NONE',  ( 2.060812052271002059, -12.52766984582000021, -317.0792622552969533 ) ) ;
#8553 = DIRECTION ( 'NONE',  ( 0.9848077530122130163, 0.000000000000000000, 0.1736481776669023813 ) ) ;
#8554 = CARTESIAN_POINT ( 'NONE',  ( -17.18550143358999449, -2.500000000000000000, -495.8459145668000474 ) ) ;
#8555 = VERTEX_POINT ( 'NONE', #1809 ) ;
#8556 = CARTESIAN_POINT ( 'NONE',  ( -8.548650239411999863, -10.26553531915999962, 190.0000000000000000 ) ) ;
#8557 = AXIS2_PLACEMENT_3D ( 'NONE', #5062, #9267, #2754 ) ;
#8558 = CARTESIAN_POINT ( 'NONE',  ( -14.04520818109275382, -8.909665382566954506, 319.0000000000003979 ) ) ;
#8559 = VERTEX_POINT ( 'NONE', #90 ) ;
#8560 = CARTESIAN_POINT ( 'NONE',  ( -0.7125182177439003395, -12.50545814267000644, 191.1197171614399792 ) ) ;
#8561 = VERTEX_POINT ( 'NONE', #5075 ) ;
#8562 = CARTESIAN_POINT ( 'NONE',  ( -39.23786858994942151, -9.000000000000001776, -387.8670522075712483 ) ) ;
#8563 = CARTESIAN_POINT ( 'NONE',  ( -46.74071243419621169, -9.500000000000001776, -414.3237589990241077 ) ) ;
#8564 = CARTESIAN_POINT ( 'NONE',  ( 4.466162596268001828, 12.19410025049000446, 191.1197171614399792 ) ) ;
#8565 = CIRCLE ( 'NONE', #10125, 0.5000000000000074385 ) ;
#8566 = CARTESIAN_POINT ( 'NONE',  ( -0.5973619912582514013, -7.470029452637001022, -434.3275123593290914 ) ) ;
#8567 = EDGE_CURVE ( 'NONE', #8110, #8301, #452, .T. ) ;
#8568 = CARTESIAN_POINT ( 'NONE',  ( -7.636686903722000430, 10.40663048292000070, -302.5071922382879279 ) ) ;
#8569 = CARTESIAN_POINT ( 'NONE',  ( -16.37943014210002346, -7.176468652514003566, 318.8802828394900644 ) ) ;
#8570 = CARTESIAN_POINT ( 'NONE',  ( 16.76545246634000108, -2.037063237379999947, -314.8616023057000461 ) ) ;
#8571 = EDGE_CURVE ( 'NONE', #6443, #5121, #8236, .T. ) ;
#8572 = CARTESIAN_POINT ( 'NONE',  ( -1.419551022038999966, 10.09154694854999867, 314.4150829855000211 ) ) ;
#8573 = VERTEX_POINT ( 'NONE', #10127 ) ;
#8574 = CARTESIAN_POINT ( 'NONE',  ( 18.69235161570000159, -1.652152683404002342, 190.0071920248299477 ) ) ;
#8575 = VERTEX_POINT ( 'NONE', #3017 ) ;
#8576 = CARTESIAN_POINT ( 'NONE',  ( -43.65370867118748777, -7.500000000000000000, -412.6743931307942717 ) ) ;
#8577 = DIRECTION ( 'NONE',  ( 0.000000000000000000, -1.000000000000000000, 0.000000000000000000 ) ) ;
#8578 = DIRECTION ( 'NONE',  ( -0.9712267471052594692, 0.000000000000000000, -0.2381566831044984178 ) ) ;
#8579 = DIRECTION ( 'NONE',  ( 0.9968876850330226080, 0.000000000000000000, -0.07883491250392217486 ) ) ;
#8580 = CARTESIAN_POINT ( 'NONE',  ( -10.25126250535807770, -10.00000007971003235, 314.9999999999999432 ) ) ;
#8581 = CARTESIAN_POINT ( 'NONE',  ( -4.603216684274966219, -9.141664750100051862, -315.0000000000000568 ) ) ;
#8582 = CYLINDRICAL_SURFACE ( 'NONE', #6949, 0.5000000000000004441 ) ;
#8583 = DIRECTION ( 'NONE',  ( 0.000000000000000000, -1.000000000000000000, 0.000000000000000000 ) ) ;
#8584 = ADVANCED_FACE ( 'NONE', ( #547 ), #2719, .F. ) ;
#8585 = DIRECTION ( 'NONE',  ( 0.000000000000000000, 1.000000000000000000, 0.000000000000000000 ) ) ;
#8586 = CARTESIAN_POINT ( 'NONE',  ( -9.619051408962835836, 7.822710805390641120, -315.0000000000000568 ) ) ;
#8587 = CARTESIAN_POINT ( 'NONE',  ( 15.60615175339998473, 6.374933892835006333, 190.0071920248299477 ) ) ;
#8588 = DIRECTION ( 'NONE',  ( -0.9942380540931625710, 0.000000000000000000, -0.1071946444233179835 ) ) ;
#8589 = CARTESIAN_POINT ( 'NONE',  ( 3.698987565691999713, -11.29118203779999874, -317.5000000000000000 ) ) ;
#8590 = CARTESIAN_POINT ( 'NONE',  ( -2.375181255485324439, -9.500000000000001776, -406.0201668106497550 ) ) ;
#8591 = CARTESIAN_POINT ( 'NONE',  ( -44.74071243416544519, -1.734723475976807094E-15, -4.823758999047855767 ) ) ;
#8592 = CARTESIAN_POINT ( 'NONE',  ( 15.43580712988967107, -3.955371400427518669, 315.0000000000000568 ) ) ;
#8593 = CARTESIAN_POINT ( 'NONE',  ( 12.21495827233999876, 7.290170534263999969, -314.4150829855000211 ) ) ;
#8594 = VECTOR ( 'NONE', #2085, 1000.000000000000227 ) ;
#8595 = DIRECTION ( 'NONE',  ( 0.000000000000000000, -1.000000000000000000, 0.000000000000000000 ) ) ;
#8596 = FILL_AREA_STYLE_COLOUR ( '', #1381 ) ;
#8597 = ADVANCED_FACE ( 'NONE', ( #7108 ), #7987, .F. ) ;
#8598 = DIRECTION ( 'NONE',  ( 0.2951854283188045658, 0.000000000000000000, -0.9554399839384175586 ) ) ;
#8599 = ORIENTED_EDGE ( 'NONE', *, *, #4128, .F. ) ;
#8600 = CARTESIAN_POINT ( 'NONE',  ( 12.29114107644999443, 8.620527874443991934, -317.4928077629770087 ) ) ;
#8601 = CARTESIAN_POINT ( 'NONE',  ( -20.06802617119998899, 0.4069525832283997779, -317.0792622552969533 ) ) ;
#8602 = PRODUCT ( 'Counter Blade', 'Counter Blade', '', ( #6451 ) ) ;
#8603 = CIRCLE ( 'NONE', #891, 5.000000000000004441 ) ;
#8604 = CARTESIAN_POINT ( 'NONE',  ( -85.79375217459825365, -2.500000000000000000, -343.3529193039154279 ) ) ;
#8605 = CARTESIAN_POINT ( 'NONE',  ( 1.831806507035697473, 9.955740905498860371, -314.5031779949862880 ) ) ;
#8606 = ORIENTED_EDGE ( 'NONE', *, *, #5460, .F. ) ;
#8607 = CARTESIAN_POINT ( 'NONE',  ( 4.792833739245000224, -11.13811509850999926, 190.0000000000000000 ) ) ;
#8608 = FACE_OUTER_BOUND ( 'NONE', #2737, .T. ) ;
#8609 = ADVANCED_FACE ( 'NONE', ( #252 ), #3881, .F. ) ;
#8610 = EDGE_LOOP ( 'NONE', ( #3517, #7362, #2648, #6848 ) ) ;
#8611 = CARTESIAN_POINT ( 'NONE',  ( -19.99999036626000048, -4.642009783819999925E-09, -316.5000000000000000 ) ) ;
#8612 = EDGE_LOOP ( 'NONE', ( #2993, #715 ) ) ;
#8613 = CARTESIAN_POINT ( 'NONE',  ( -77.77979771402830522, -2.500000000000000000, -385.9384419754180158 ) ) ;
#8614 = CARTESIAN_POINT ( 'NONE',  ( 10.11757849520999031, -9.598459870364994373, -302.5071922382879279 ) ) ;
#8615 = CARTESIAN_POINT ( 'NONE',  ( -1.873948611771682149, -12.50000000000000000, -349.2478646809681777 ) ) ;
#8616 = EDGE_CURVE ( 'NONE', #830, #4372, #3766, .T. ) ;
#8617 = CARTESIAN_POINT ( 'NONE',  ( -79.04021210711869116, -7.500000000000000000, -328.4066924704651456 ) ) ;
#8618 =( NAMED_UNIT ( * ) SI_UNIT ( $, .STERADIAN. ) SOLID_ANGLE_UNIT ( ) );
#8619 = EDGE_CURVE ( 'NONE', #2293, #6915, #5985, .T. ) ;
#8620 = CARTESIAN_POINT ( 'NONE',  ( 17.50000000000002487, 1.995060298004523415E-08, 314.4999385900306947 ) ) ;
#8621 = CARTESIAN_POINT ( 'NONE',  ( -12.24957049234000728, -9.976523051824997879, 319.5792614743400009 ) ) ;
#8622 = CARTESIAN_POINT ( 'NONE',  ( 17.12243801299000268, -0.5826713957640000663, -314.8616023057000461 ) ) ;
#8623 = CARTESIAN_POINT ( 'NONE',  ( 1.266716818501000041, 9.650794245151999462, 314.8616023057000461 ) ) ;
#8624 = ORIENTED_EDGE ( 'NONE', *, *, #5879, .T. ) ;
#8625 = CARTESIAN_POINT ( 'NONE',  ( 18.86316454545999832, 0.4769905026584997931, 190.0071920248299477 ) ) ;
#8626 = VERTEX_POINT ( 'NONE', #6856 ) ;
#8627 = CARTESIAN_POINT ( 'NONE',  ( -1.170813146951170225, -7.466834095521711845, -434.4923879807246294 ) ) ;
#8628 = B_SPLINE_CURVE_WITH_KNOTS ( 'NONE', 3,
 ( #6563, #3181, #4644, #6622, #9845, #6455, #561, #2483, #5440, #4589, #8717, #4948, #9899, #7914, #510, #3783, #1360, #9532, #2172, #3835, #227, #4362, #1130, #2645, #7479, #277, #7580, #5913, #1838, #3556, #1783, #6728, #6672, #6837, #330, #915, #2591, #3607, #10106, #2535, #10058, #1890, #6890, #4998, #2748, #6786, #6016, #5802 ),
 .UNSPECIFIED., .F., .F.,
 ( 4, 1, 1, 1, 1, 1, 1, 1, 1, 1, 1, 1, 1, 1, 1, 1, 1, 1, 1, 1, 1, 1, 1, 1, 1, 1, 1, 1, 1, 1, 1, 1, 1, 1, 1, 1, 1, 1, 1, 1, 1, 1, 1, 1, 1, 4 ),
 ( 0.000000000000000000, 0.02222222222221999915, 0.04444444444443999831, 0.06666666666666999641, 0.08888888888889000250, 0.1111111111111000027, 0.1333333333332999970, 0.1555555555555999947, 0.1777777777777999890, 0.2000000000000000111, 0.2222222222222000054, 0.2444444444443999997, 0.2666666666666999697, 0.2888888888889000195, 0.3111111111111000138, 0.3333333333333000081, 0.3555555555556000336, 0.3777777777777999724, 0.4000000000000000222, 0.4222222222221999610, 0.4444444444444000109, 0.4666666666666999808, 0.4888888888889000306, 0.5111111111110999694, 0.5333333333333000192, 0.5555555555555999891, 0.5777777777778000390, 0.5999999999999999778, 0.6222222222222000276, 0.6444444444443999664, 0.6666666666667000474, 0.6888888888888999862, 0.7111111111111000360, 0.7333333333333000859, 0.7555555555556000558, 0.7777777777777999946, 0.8000000000000000444, 0.8222222222221999832, 0.8444444444443999220, 0.8666666666667000030, 0.8888888888888999418, 0.9111111111110999916, 0.9333333333333000414, 0.9555555555556000114, 0.9777777777778000612, 1.000000000000000000 ),
 .UNSPECIFIED. ) ;
#8629 = DIRECTION ( 'NONE',  ( 0.9627072927120896573, 0.1321637200909031584, 0.2360665576711206692 ) ) ;
#8630 = VECTOR ( 'NONE', #948, 1000.000000000000000 ) ;
#8631 = ADVANCED_FACE ( 'NONE', ( #2767, #9466, #7158 ), #498, .F. ) ;
#8632 = VERTEX_POINT ( 'NONE', #2162 ) ;
#8633 = CARTESIAN_POINT ( 'NONE',  ( -47.11589368967775471, -9.500000000000001776, -410.8439258096980780 ) ) ;
#8634 = CARTESIAN_POINT ( 'NONE',  ( 0.000000000000000000, 0.000000000000000000, 0.000000000000000000 ) ) ;
#8635 = CARTESIAN_POINT ( 'NONE',  ( -16.82367287970800973, 1.353209159721973309, 315.0000000000000000 ) ) ;
#8636 = CARTESIAN_POINT ( 'NONE',  ( -17.50000000000000000, -3.147917160613439321E-08, 315.0000000000000000 ) ) ;
#8637 = CARTESIAN_POINT ( 'NONE',  ( -12.16683899257771806, -6.621314373557687816, -315.0000000000000568 ) ) ;
#8638 = CARTESIAN_POINT ( 'NONE',  ( -0.6524225759890166509, -2.520141586570888492, -434.5249754051499167 ) ) ;
#8639 = CARTESIAN_POINT ( 'NONE',  ( -2.000000000000000000, -10.50000000000000000, -409.5000000000000000 ) ) ;
#8640 = STYLED_ITEM ( 'NONE', ( #2043 ), #8977 ) ;
#8641 = CARTESIAN_POINT ( 'NONE',  ( -7.666814856007332146, -6.251400993695000352, -437.4143429429252592 ) ) ;
#8642 = CARTESIAN_POINT ( 'NONE',  ( -4.648899539349732990, 9.134382686408034857, -315.0000000000000000 ) ) ;
#8643 = CARTESIAN_POINT ( 'NONE',  ( -14.19899178590998190, 7.472503199908998361, 190.0071920248299477 ) ) ;
#8644 = LINE ( 'NONE', #1290, #3848 ) ;
#8645 = AXIS2_PLACEMENT_3D ( 'NONE', #8551, #8401, #4327 ) ;
#8646 = ORIENTED_EDGE ( 'NONE', *, *, #2698, .F. ) ;
#8647 = CARTESIAN_POINT ( 'NONE',  ( -81.20226567874760804, -2.500000000000000000, -347.7024309728756748 ) ) ;
#8648 = AXIS2_PLACEMENT_3D ( 'NONE', #1285, #7098, #9508 ) ;
#8649 = CIRCLE ( 'NONE', #10546, 0.5000000000000004441 ) ;
#8650 = DIRECTION ( 'NONE',  ( -0.9942380540931650135, 0.000000000000000000, -0.1071946444232960011 ) ) ;
#8651 = FILL_AREA_STYLE ('',( #7002 ) ) ;
#8652 = CARTESIAN_POINT ( 'NONE',  ( 16.35728328174216273, -2.567538628164302228, 315.0000000000000568 ) ) ;
#8653 = CARTESIAN_POINT ( 'NONE',  ( 6.419414596134000561, 9.427679607337001499, -314.4150829855000211 ) ) ;
#8654 = CARTESIAN_POINT ( 'NONE',  ( -3.206493966914822025, -9.870881096968846080, 314.4999451744449743 ) ) ;
#8655 = CARTESIAN_POINT ( 'NONE',  ( 11.06499621481999895, 9.965574156584002807, 320.0770942683900557 ) ) ;
#8656 = CARTESIAN_POINT ( 'NONE',  ( -19.68871134463705985, -9.000000000000001776, -416.4361005590961327 ) ) ;
#8657 = LINE ( 'NONE', #5225, #9995 ) ;
#8658 = ORIENTED_EDGE ( 'NONE', *, *, #1891, .T. ) ;
#8659 = VECTOR ( 'NONE', #8523, 1000.000000000000000 ) ;
#8660 = CARTESIAN_POINT ( 'NONE',  ( -0.2332652941728000917, 12.09631257874000099, -317.5770954168139610 ) ) ;
#8661 = CARTESIAN_POINT ( 'NONE',  ( -20.05669107747999291, 0.5612988332226998001, -317.0792622552969533 ) ) ;
#8662 = CARTESIAN_POINT ( 'NONE',  ( -14.96977070983867009, -8.000000000000000000, -385.2505660326773409 ) ) ;
#8663 = EDGE_LOOP ( 'NONE', ( #1273, #9029, #8658, #8037 ) ) ;
#8664 = CARTESIAN_POINT ( 'NONE',  ( 14.55942669488976549, 5.453671309400857758, -314.5801547934441942 ) ) ;
#8665 = ORIENTED_EDGE ( 'NONE', *, *, #5482, .T. ) ;
#8666 = CARTESIAN_POINT ( 'NONE',  ( -51.41224207513305799, -12.00000000000000000, -371.0859316413308306 ) ) ;
#8667 =( GEOMETRIC_REPRESENTATION_CONTEXT ( 3 ) GLOBAL_UNCERTAINTY_ASSIGNED_CONTEXT ( ( #237 ) ) GLOBAL_UNIT_ASSIGNED_CONTEXT ( ( #4711, #5558, #9115 ) ) REPRESENTATION_CONTEXT ( 'NONE', 'WORKASPACE' ) );
#8668 = CARTESIAN_POINT ( 'NONE',  ( -17.50000000000000711, 8.653878165429867666E-10, 190.0000000000001137 ) ) ;
#8669 = EDGE_LOOP ( 'NONE', ( #7490, #1798, #8851, #2070 ) ) ;
#8670 = CARTESIAN_POINT ( 'NONE',  ( -72.90663470096859555, -2.500000000000000000, -371.7168990827444190 ) ) ;
#8671 = ORIENTED_EDGE ( 'NONE', *, *, #5900, .T. ) ;
#8672 = DIRECTION ( 'NONE',  ( -0.2951854283188049544, 0.000000000000000000, 0.9554399839384176696 ) ) ;
#8673 = CARTESIAN_POINT ( 'NONE',  ( 14.73495828939998731, -7.957952820716998055, -302.4229045757450081 ) ) ;
#8674 = CARTESIAN_POINT ( 'NONE',  ( -1.873948611771682149, -8.000000000000000000, -349.2478646809681777 ) ) ;
#8675 = LINE ( 'NONE', #1265, #7179 ) ;
#8676 = PRESENTATION_STYLE_ASSIGNMENT (( #10349 ) ) ;
#8677 = CARTESIAN_POINT ( 'NONE',  ( 16.06615879071999231, 5.957812395457000143, -302.5071922382879279 ) ) ;
#8678 = CARTESIAN_POINT ( 'NONE',  ( -3.213253768582002845, -12.43294388789000138, 319.5792614743400009 ) ) ;
#8679 = CARTESIAN_POINT ( 'NONE',  ( 13.37260572687999982, -6.041714840053000302, -314.8616023057000461 ) ) ;
#8680 = CARTESIAN_POINT ( 'NONE',  ( -15.60185585328000002, 4.689707898928999974, 314.4150829855000211 ) ) ;
#8681 = ORIENTED_EDGE ( 'NONE', *, *, #9093, .T. ) ;
#8682 = CARTESIAN_POINT ( 'NONE',  ( 18.85089486759000010, -0.8058634873976002755, 190.0071920248299477 ) ) ;
#8683 = CARTESIAN_POINT ( 'NONE',  ( -8.771473555299991176, 11.23637119458999223, 318.8802828394900644 ) ) ;
#8684 = PRODUCT_DEFINITION ( 'UNKNOWN', '', #281, #4958 ) ;
#8685 = CARTESIAN_POINT ( 'NONE',  ( -101.0297452788102817, -7.500000000000000000, -342.4231267849074811 ) ) ;
#8686 = CARTESIAN_POINT ( 'NONE',  ( -2.000000000000000000, 2.500000000000000000, -409.5000000000000000 ) ) ;
#8687 = DIRECTION ( 'NONE',  ( 0.000000000000000000, -1.000000000000000000, 0.000000000000000000 ) ) ;
#8688 = CARTESIAN_POINT ( 'NONE',  ( 14.79012398734008293, -1.483731117706880154, 315.0000000000001705 ) ) ;
#8689 = CARTESIAN_POINT ( 'NONE',  ( -4.461988713456979561, -9.163769885065249809, -314.9999999999999432 ) ) ;
#8690 = CYLINDRICAL_SURFACE ( 'NONE', #8648, 10.00000000000000533 ) ;
#8691 = FACE_OUTER_BOUND ( 'NONE', #10340, .T. ) ;
#8692 = DIRECTION ( 'NONE',  ( -0.4712473909295827323, 0.000000000000000000, 0.8820010751365675583 ) ) ;
#8693 = CARTESIAN_POINT ( 'NONE',  ( 8.636340573252622832, 8.171206817651022192, -315.0000000000000000 ) ) ;
#8694 = CARTESIAN_POINT ( 'NONE',  ( 16.73002466287002576, 6.274001814427998980, 189.9229057364800042 ) ) ;
#8695 = CARTESIAN_POINT ( 'NONE',  ( 16.56522183954892924, 3.263825208519234078, 314.4999489731222297 ) ) ;
#8696 = ADVANCED_FACE ( 'NONE', ( #5373 ), #4686, .T. ) ;
#8697 = AXIS2_PLACEMENT_3D ( 'NONE', #9476, #7860, #506 ) ;
#8698 = ORIENTED_EDGE ( 'NONE', *, *, #7244, .T. ) ;
#8699 = CARTESIAN_POINT ( 'NONE',  ( 15.28484891664999878, -6.814525346632999359, -317.5000000000000000 ) ) ;
#8700 = CARTESIAN_POINT ( 'NONE',  ( -1.658528026434172631, -7.334393795902656166, -435.0029499069592589 ) ) ;
#8701 = DIRECTION ( 'NONE',  ( 1.000000000000000000, 0.000000000000000000, 0.000000000000000000 ) ) ;
#8702 = CARTESIAN_POINT ( 'NONE',  ( 3.970161185191127817, -9.235879793686278205, 315.0000000000000000 ) ) ;
#8703 = CARTESIAN_POINT ( 'NONE',  ( 13.44085293541000148, 6.266915263066000108, -314.6383426456000052 ) ) ;
#8704 = ADVANCED_FACE ( 'NONE', ( #608 ), #3180, .T. ) ;
#8705 = DIRECTION ( 'NONE',  ( -1.000000000000000000, 0.000000000000000000, 0.000000000000000000 ) ) ;
#8706 = VECTOR ( 'NONE', #3805, 1000.000000000000000 ) ;
#8707 = EDGE_CURVE ( 'NONE', #8266, #3792, #8925, .T. ) ;
#8708 = CARTESIAN_POINT ( 'NONE',  ( -17.29814430729002339, 5.659421966102000212, 320.0770942683900557 ) ) ;
#8709 = CARTESIAN_POINT ( 'NONE',  ( -0.4971732199403511299, -2.511415353335999967, -434.1478469224045966 ) ) ;
#8710 = ORIENTED_EDGE ( 'NONE', *, *, #8849, .F. ) ;
#8711 = CARTESIAN_POINT ( 'NONE',  ( 14.69255688194000520, 7.987735679832996816, -317.5770954168139610 ) ) ;
#8712 = CARTESIAN_POINT ( 'NONE',  ( -12.61362476840000113, -9.241140244908006451, -317.5770954168139610 ) ) ;
#8713 = DIRECTION ( 'NONE',  ( 0.000000000000000000, 1.000000000000000000, 0.000000000000000000 ) ) ;
#8714 = MANIFOLD_SOLID_BREP ( 'Stock-MAS-686-1', #4203 ) ;
#8715 = CARTESIAN_POINT ( 'NONE',  ( -14.57677553938588844, 5.476482737502800013, -314.5817494731896318 ) ) ;
#8716 = VERTEX_POINT ( 'NONE', #3282 ) ;
#8717 = CARTESIAN_POINT ( 'NONE',  ( -15.66827725153000017, 6.479182156166999995, 190.0000000000000000 ) ) ;
#8718 = DIRECTION ( 'NONE',  ( 0.000000000000000000, -1.000000000000000000, 0.000000000000000000 ) ) ;
#8719 = EDGE_CURVE ( 'NONE', #726, #10547, #2266, .T. ) ;
#8720 = VERTEX_POINT ( 'NONE', #8067 ) ;
#8721 = CARTESIAN_POINT ( 'NONE',  ( 19.99984272814741715, 0.5882336804855479162, -316.5000000000004547 ) ) ;
#8722 = ORIENTED_EDGE ( 'NONE', *, *, #8719, .T. ) ;
#8723 = CARTESIAN_POINT ( 'NONE',  ( -14.00164231856462926, -5.362560482542400919, 315.0000000000000000 ) ) ;
#8724 = CARTESIAN_POINT ( 'NONE',  ( -13.67213454565999875, -8.648884013374997792, -302.4229045757450081 ) ) ;
#8725 = CARTESIAN_POINT ( 'NONE',  ( -63.11273421720001409, -2.500000000000000000, -415.2750182148000135 ) ) ;
#8726 =( BOUNDED_SURFACE ( )  B_SPLINE_SURFACE ( 3, 1, ( 
 ( #8164, #645 ),
 ( #3166, #2198 ),
 ( #8912, #2252 ),
 ( #1557, #9776 ),
 ( #7198, #8106 ),
 ( #7307, #5467 ),
 ( #2417, #5683 ) ),
 .UNSPECIFIED., .F., .F., .T. ) 
 B_SPLINE_SURFACE_WITH_KNOTS ( ( 4, 3, 4 ),
 ( 2, 2 ),
 ( 0.006576891565977040048, 0.5000000000000000000, 0.9934231084340230389 ),
 ( 0.000000000000000000, 1.000000000000000000 ),
 .UNSPECIFIED. ) 
 GEOMETRIC_REPRESENTATION_ITEM ( )  RATIONAL_B_SPLINE_SURFACE ( (
 ( 0.9922222087809811075, 0.9922222087809811075),
 ( 0.8003084355045908538, 0.8003084355045908538),
 ( 0.8029010325775970403, 0.8029010325775970403),
 ( 1.000000000000000000, 1.000000000000000000),
 ( 0.8029010325775969292, 0.8029010325775969292),
 ( 0.8003084355045906317, 0.8003084355045906317),
 ( 0.9922222087809811075, 0.9922222087809811075) ) ) 
 REPRESENTATION_ITEM ( '' )  SURFACE ( )  );
#8727 = CARTESIAN_POINT ( 'NONE',  ( -0.5929282851181935099, -7.526005961551003764, -434.8233273616743872 ) ) ;
#8728 = CIRCLE ( 'NONE', #4111, 15.50000000000001421 ) ;
#8729 = CARTESIAN_POINT ( 'NONE',  ( 1.914578617915998704, 11.33709939001001032, -302.5071922382879279 ) ) ;
#8730 = CARTESIAN_POINT ( 'NONE',  ( -6.472425350819999146, -11.83301930295000126, 318.8802828394900644 ) ) ;
#8731 = ORIENTED_EDGE ( 'NONE', *, *, #2712, .T. ) ;
#8732 = CARTESIAN_POINT ( 'NONE',  ( -13.44085293541000148, -6.266915263066000108, -314.6383426456000052 ) ) ;
#8733 = CARTESIAN_POINT ( 'NONE',  ( -6.514686351705899270, -2.852628117829832277, -436.2336205443476729 ) ) ;
#8734 = ORIENTED_EDGE ( 'NONE', *, *, #1223, .T. ) ;
#8735 = CARTESIAN_POINT ( 'NONE',  ( -18.14082875322000277, -3.150077164920001671, 190.0071920248299477 ) ) ;
#8736 = CARTESIAN_POINT ( 'NONE',  ( -1.813125098999968543, -7.427867185880000278, -434.7536662776001322 ) ) ;
#8737 = DIRECTION ( 'NONE',  ( -0.2868111944991166840, 0.000000000000000000, -0.9579871286765756500 ) ) ;
#8738 = EDGE_CURVE ( 'NONE', #8053, #8216, #1723, .T. ) ;
#8739 = AXIS2_PLACEMENT_3D ( 'NONE', #3931, #8871, #8813 ) ;
#8740 = EDGE_LOOP ( 'NONE', ( #4594, #10495 ) ) ;
#8741 = CARTESIAN_POINT ( 'NONE',  ( -3.932702496464000497, -9.868769537474999964, 314.4150829855000211 ) ) ;
#8742 = CARTESIAN_POINT ( 'NONE',  ( -38.59226537204000351, -2.500000000000000000, -500.7880554352000217 ) ) ;
#8743 = CARTESIAN_POINT ( 'NONE',  ( -6.594989095229207621, -7.500000000000000000, -526.5005977704149700 ) ) ;
#8744 = AXIS2_PLACEMENT_3D ( 'NONE', #8330, #1726, #1071 ) ;
#8745 = CARTESIAN_POINT ( 'NONE',  ( -8.517086849895166623, -8.210518282650744126, -314.9999999999999432 ) ) ;
#8746 = CARTESIAN_POINT ( 'NONE',  ( -14.92529112109648004, -4.159649519892460567, -438.6682410860930759 ) ) ;
#8747 = ORIENTED_EDGE ( 'NONE', *, *, #2024, .T. ) ;
#8748 = CARTESIAN_POINT ( 'NONE',  ( -27.98005464532998232, -9.500000000000001776, -417.3300389808354680 ) ) ;
#8749 = CARTESIAN_POINT ( 'NONE',  ( -8.673912564134326431, 8.158689640371338925, -315.0000000000000000 ) ) ;
#8750 = ADVANCED_FACE ( 'NONE', ( #3232 ), #8138, .T. ) ;
#8751 = CARTESIAN_POINT ( 'NONE',  ( -20.08953225942999765, 0.1031351683529000418, 190.4207385301700128 ) ) ;
#8752 = CARTESIAN_POINT ( 'NONE',  ( 17.33327037445099705, 2.718757125457364851E-08, -314.6666037066913759 ) ) ;
#8753 = AXIS2_PLACEMENT_3D ( 'NONE', #3506, #7036, #5303 ) ;
#8754 = CARTESIAN_POINT ( 'NONE',  ( -12.33668477992999968, -8.731648389349999206, -317.5000000000000000 ) ) ;
#8755 = CONICAL_SURFACE ( 'NONE', #3782, 3.400000000000014122, 0.7853981633975372079 ) ;
#8756 = EDGE_CURVE ( 'NONE', #4350, #6593, #8015, .T. ) ;
#8757 = DIRECTION ( 'NONE',  ( 0.000000000000000000, -1.000000000000000000, 0.000000000000000000 ) ) ;
#8758 = APPLICATION_PROTOCOL_DEFINITION ( 'draft international standard', 'automotive_design', 1998, #4695 ) ;
#8759 = CARTESIAN_POINT ( 'NONE',  ( 7.529172669043764365, -8.513076715957524243, 315.0000000000000000 ) ) ;
#8760 = EDGE_CURVE ( 'NONE', #3792, #7526, #5901, .T. ) ;
#8761 = CARTESIAN_POINT ( 'NONE',  ( -6.388932193737000276, 8.746770244069999478, -315.0848619657999734 ) ) ;
#8762 = CARTESIAN_POINT ( 'NONE',  ( -37.45790571715708239, -9.000000000000001776, -422.6951089172942488 ) ) ;
#8763 = CARTESIAN_POINT ( 'NONE',  ( -19.56036991370999800, -0.5261966905397996719, 320.0770942683900557 ) ) ;
#8764 = DIRECTION ( 'NONE',  ( 0.9942380540931650135, 0.000000000000000000, 0.1071946444232960011 ) ) ;
#8765 = CARTESIAN_POINT ( 'NONE',  ( -1.419469786162590674, -2.618831809747000694, -434.7498648015279059 ) ) ;
#8766 = VERTEX_POINT ( 'NONE', #1673 ) ;
#8767 = CARTESIAN_POINT ( 'NONE',  ( 10.31351018857999513, 10.27238149472999851, -317.5770954168139610 ) ) ;
#8768 = DIRECTION ( 'NONE',  ( -0.5828070674935414974, 0.000000000000000000, -0.8126105599114366029 ) ) ;
#8769 = AXIS2_PLACEMENT_3D ( 'NONE', #8662, #2169, #10236 ) ;
#8770 = CARTESIAN_POINT ( 'NONE',  ( 0.000000000000000000, -10.54711710274999881, -315.0000000000000000 ) ) ;
#8771 = EDGE_CURVE ( 'NONE', #3758, #8913, #4146, .T. ) ;
#8772 = CARTESIAN_POINT ( 'NONE',  ( -15.16362200326591569, -2.500000000000000000, -437.6963039377973246 ) ) ;
#8773 = VERTEX_POINT ( 'NONE', #4946 ) ;
#8774 = CARTESIAN_POINT ( 'NONE',  ( -16.39561153668570270, -3.420321068896106986, -314.5539561507840176 ) ) ;
#8775 = EDGE_LOOP ( 'NONE', ( #671, #9232, #3532, #6458, #3666, #8665, #6806, #3290 ) ) ;
#8776 = DIRECTION ( 'NONE',  ( 0.8820010751365678914, 0.000000000000000000, 0.4712473909295818442 ) ) ;
#8777 = ORIENTED_EDGE ( 'NONE', *, *, #7911, .F. ) ;
#8778 = CARTESIAN_POINT ( 'NONE',  ( -12.45718924559404250, -6.445992642206118006, 315.0000000000000568 ) ) ;
#8779 = CARTESIAN_POINT ( 'NONE',  ( -18.18877801098002323, -4.514014122889999037, -302.4229045757450081 ) ) ;
#8780 = DIRECTION ( 'NONE',  ( 0.000000000000000000, -1.000000000000000000, 0.000000000000000000 ) ) ;
#8781 = AXIS2_PLACEMENT_3D ( 'NONE', #2952, #5416, #1391 ) ;
#8782 = B_SPLINE_CURVE_WITH_KNOTS ( 'NONE', 3,
 ( #1778, #2530, #10053, #6723, #5047, #4254, #9255, #4199, #9140, #5798, #1884, #4944, #61 ),
 .UNSPECIFIED., .F., .F.,
 ( 4, 1, 1, 1, 1, 1, 1, 1, 1, 1, 4 ),
 ( 0.000000000000000000, 0.08333333333333001192, 0.1666666666667000196, 0.2500000000000000000, 0.3333333333333000081, 0.5000000000000000000, 0.6666666666667000474, 0.7500000000000000000, 0.8333333333333000637, 0.9166666666667000474, 1.000000000000000000 ),
 .UNSPECIFIED. ) ;
#8783 = CARTESIAN_POINT ( 'NONE',  ( -3.382256884648001893, 11.91212135210998824, -302.4229045757450081 ) ) ;
#8784 = PRODUCT ( 'Handle Mounting Bracket', 'Handle Mounting Bracket', '', ( #1460 ) ) ;
#8785 = CARTESIAN_POINT ( 'NONE',  ( -1002.398135702230206, -2.500000000000000000, -618.0215964952759577 ) ) ;
#8786 = EDGE_LOOP ( 'NONE', ( #2789, #7931, #10200, #8838 ) ) ;
#8787 = CARTESIAN_POINT ( 'NONE',  ( -15.23514566747999943, -4.427644513407000382, -314.8616023057000461 ) ) ;
#8788 = CARTESIAN_POINT ( 'NONE',  ( -5.561800649038728395, -2.795979873486618139, -435.9619414120115266 ) ) ;
#8789 = TOROIDAL_SURFACE ( 'NONE', #5349, 12.00000000000000000, 0.5000000000000000000 ) ;
#8790 = VERTEX_POINT ( 'NONE', #7370 ) ;
#8791 = CARTESIAN_POINT ( 'NONE',  ( 8.887010007670999912, -10.76703833147000822, 189.9229057364800042 ) ) ;
#8792 = CARTESIAN_POINT ( 'NONE',  ( -18.68747751655417133, 4.479206664350980027, 190.9999999999996589 ) ) ;
#8793 = DIRECTION ( 'NONE',  ( 0.9958031466069877657, 0.000000000000000000, 0.09152099872500310540 ) ) ;
#8794 = EDGE_LOOP ( 'NONE', ( #7072, #10270, #1447, #5177 ) ) ;
#8795 = CIRCLE ( 'NONE', #57, 3.999999999999996447 ) ;
#8796 = ORIENTED_EDGE ( 'NONE', *, *, #4591, .T. ) ;
#8797 = CARTESIAN_POINT ( 'NONE',  ( -13.44085293541000148, -6.266915263066000108, 314.6383426456000052 ) ) ;
#8798 = FACE_BOUND ( 'NONE', #8740, .T. ) ;
#8799 = CARTESIAN_POINT ( 'NONE',  ( 16.84305512206999822, 5.298470530761999697, 320.0000000000000000 ) ) ;
#8800 = CARTESIAN_POINT ( 'NONE',  ( -4.753602499919002078, -11.02326831536999840, 319.9928079742500131 ) ) ;
#8801 = CARTESIAN_POINT ( 'NONE',  ( 19.99996733365995283, 0.3063832366037737009, 319.0000000000005116 ) ) ;
#8802 = DIRECTION ( 'NONE',  ( 0.000000000000000000, 1.000000000000000000, 0.000000000000000000 ) ) ;
#8803 = FACE_BOUND ( 'NONE', #6567, .T. ) ;
#8804 = ORIENTED_EDGE ( 'NONE', *, *, #9542, .F. ) ;
#8805 = DIRECTION ( 'NONE',  ( -0.4712473909295860630, 0.000000000000000000, 0.8820010751365656709 ) ) ;
#8806 = CARTESIAN_POINT ( 'NONE',  ( 13.71790339694999439, 8.616951602761004025, 189.9229057364800042 ) ) ;
#8807 = CARTESIAN_POINT ( 'NONE',  ( 17.50000000000000711, -8.653864165198663120E-10, 189.9999999999999432 ) ) ;
#8808 = CARTESIAN_POINT ( 'NONE',  ( 10.00000000000000000, -2.500000000000000000, -317.5000000000000000 ) ) ;
#8809 = EDGE_CURVE ( 'NONE', #2603, #8268, #2822, .T. ) ;
#8810 = CARTESIAN_POINT ( 'NONE',  ( 11.93437769929943926, 6.745090416342686801, 315.0000000000000568 ) ) ;
#8811 = CIRCLE ( 'NONE', #4195, 15.00000000000001776 ) ;
#8812 = SHAPE_DEFINITION_REPRESENTATION ( #3130, #8468 ) ;
#8813 = DIRECTION ( 'NONE',  ( 0.000000000000000000, 0.000000000000000000, -1.000000000000000000 ) ) ;
#8814 =( BOUNDED_SURFACE ( )  B_SPLINE_SURFACE ( 3, 3, ( 
 ( #5536, #2326, #10484, #1518, #7965, #5486, #8820, #4747, #7161, #6346, #8017, #3020, #2968, #7856, #4689, #3126, #3184, #1406, #6239, #5594 ),
 ( #611, #3884, #8876, #550, #8765, #5431, #4798, #9738, #10327, #1352, #2380, #8070, #1300, #1466, #5644, #10432, #8709, #4580, #501, #714 ),
 ( #3072, #3769, #3987, #660, #9628, #2270, #7062, #3936, #9525, #6457, #7112, #10380, #7269, #2165, #4634, #7905, #6294, #9579, #2218, #7216 ),
 ( #6404, #7323, #1626, #4046, #9147, #10594, #3236, #4851, #9794, #7373, #2537, #7481, #9095, #10007, #4261, #176, #4095, #8336, #1785, #5804 ) ),
 .UNSPECIFIED., .F., .F., .F. ) 
 B_SPLINE_SURFACE_WITH_KNOTS ( ( 4, 4 ),
 ( 4, 1, 1, 1, 1, 1, 1, 1, 1, 1, 1, 1, 1, 1, 1, 1, 1, 4 ),
 ( 0.000000000000000000, 1.000000000000000000 ),
 ( 0.1929541978887999998, 0.2554811723075999796, 0.3278331352657999909, 0.3941678789460000276, 0.4549425011739000047, 0.5106931027059999906, 0.5620016754668999415, 0.6094703044461000641, 0.6536430579613999869, 0.6948991896359000275, 0.7334433934487000206, 0.7692443867375999833, 0.8015803013500999441, 0.8300487060171000131, 0.8556850663905000154, 0.8806332672557000141, 0.9057989055234000331, 0.9210247255515999765 ),
 .UNSPECIFIED. ) 
 GEOMETRIC_REPRESENTATION_ITEM ( )  RATIONAL_B_SPLINE_SURFACE ( (
 ( 1.026139272308000061, 1.026139272308000061, 1.026139272308000061, 1.026139272308000061, 1.026139272308000061, 1.026139272308000061, 1.026139272308000061, 1.026139272308000061, 1.026139272308000061, 1.026139272308000061, 1.026139272308000061, 1.026139272308000061, 1.026139272308000061, 1.026139272308000061, 1.026139272308000061, 1.026139272308000061, 1.026139272308000061, 1.026139272308000061, 1.026139272308000061, 1.026139272308000061),
 ( 0.9912869092307000640, 0.9912869092307000640, 0.9912869092307000640, 0.9912869092307000640, 0.9912869092307000640, 0.9912869092307000640, 0.9912869092307000640, 0.9912869092307000640, 0.9912869092307000640, 0.9912869092307000640, 0.9912869092307000640, 0.9912869092307000640, 0.9912869092307000640, 0.9912869092307000640, 0.9912869092307000640, 0.9912869092307000640, 0.9912869092307000640, 0.9912869092307000640, 0.9912869092307000640, 0.9912869092307000640),
 ( 0.9912869092307000640, 0.9912869092307000640, 0.9912869092307000640, 0.9912869092307000640, 0.9912869092307000640, 0.9912869092307000640, 0.9912869092307000640, 0.9912869092307000640, 0.9912869092307000640, 0.9912869092307000640, 0.9912869092307000640, 0.9912869092307000640, 0.9912869092307000640, 0.9912869092307000640, 0.9912869092307000640, 0.9912869092307000640, 0.9912869092307000640, 0.9912869092307000640, 0.9912869092307000640, 0.9912869092307000640),
 ( 1.026139272308000061, 1.026139272308000061, 1.026139272308000061, 1.026139272308000061, 1.026139272308000061, 1.026139272308000061, 1.026139272308000061, 1.026139272308000061, 1.026139272308000061, 1.026139272308000061, 1.026139272308000061, 1.026139272308000061, 1.026139272308000061, 1.026139272308000061, 1.026139272308000061, 1.026139272308000061, 1.026139272308000061, 1.026139272308000061, 1.026139272308000061, 1.026139272308000061) ) ) 
 REPRESENTATION_ITEM ( '' )  SURFACE ( )  );
#8815 = CARTESIAN_POINT ( 'NONE',  ( 17.20518503178000103, 1.389427005613000032, -314.6383426456000052 ) ) ;
#8816 = CARTESIAN_POINT ( 'NONE',  ( 19.56036306585002293, -0.5267516669946002983, 320.0770942683900557 ) ) ;
#8817 = TOROIDAL_SURFACE ( 'NONE', #9178, 12.00000000000000000, 0.5000000000000000000 ) ;
#8818 = DIRECTION ( 'NONE',  ( 0.000000000000000000, -1.000000000000000000, 0.000000000000000000 ) ) ;
#8819 = VECTOR ( 'NONE', #3768, 1000.000000000000000 ) ;
#8820 = CARTESIAN_POINT ( 'NONE',  ( -1.302538776795788555, -2.519749681487999382, -434.4904071209729182 ) ) ;
#8821 = VERTEX_POINT ( 'NONE', #4845 ) ;
#8822 = CARTESIAN_POINT ( 'NONE',  ( 16.55682536756000545, 6.456981081556999236, -317.5770954168139610 ) ) ;
#8823 = ORIENTED_CLOSED_SHELL ( 'NONE', *, #83, .F. );
#8824 = CARTESIAN_POINT ( 'NONE',  ( 19.98286815278001427, 0.4166756924005995955, -316.3802825947000201 ) ) ;
#8825 = PRESENTATION_LAYER_ASSIGNMENT (  '', '', ( #1264 ) ) ;
#8826 = AXIS2_PLACEMENT_3D ( 'NONE', #3431, #5893, #6710 ) ;
#8827 = EDGE_CURVE ( 'NONE', #9158, #7016, #8312, .T. ) ;
#8828 = ORIENTED_EDGE ( 'NONE', *, *, #4791, .T. ) ;
#8829 = DIRECTION ( 'NONE',  ( -1.000000000000000000, 0.000000000000000000, 0.000000000000000000 ) ) ;
#8830 = UNCERTAINTY_MEASURE_WITH_UNIT (LENGTH_MEASURE( 1.000000000000000082E-05 ), #10504, 'distance_accuracy_value', 'NONE');
#8831 = CARTESIAN_POINT ( 'NONE',  ( -2.000000000000000000, 2.500000000000000000, -409.5000000000000000 ) ) ;
#8832 = CARTESIAN_POINT ( 'NONE',  ( -13.85286411329785849, 6.044949306166729208, -314.5816605312646175 ) ) ;
#8834 = VERTEX_POINT ( 'NONE', #4042 ) ;
#8833 = AXIS2_PLACEMENT_3D ( 'NONE', #887, #5774, #5131 ) ;
#8835 = CARTESIAN_POINT ( 'NONE',  ( -7.251913689787720330, -9.130298775770061326, -314.5336966332658335 ) ) ;
#8836 = ORIENTED_EDGE ( 'NONE', *, *, #7709, .T. ) ;
#8837 = CYLINDRICAL_SURFACE ( 'NONE', #218, 1000.000000000000000 ) ;
#8838 = ORIENTED_EDGE ( 'NONE', *, *, #4489, .F. ) ;
#8839 = CARTESIAN_POINT ( 'NONE',  ( -11.78107618649762500, -6.828710352419061103, 315.0000000000000000 ) ) ;
#8840 = CARTESIAN_POINT ( 'NONE',  ( 18.86312040460998674, 0.4763280864498002920, -302.5071922382879279 ) ) ;
#8841 = ADVANCED_FACE ( 'NONE', ( #10590 ), #1788, .T. ) ;
#8842 = CARTESIAN_POINT ( 'NONE',  ( 3.875825478601963248, -2.500000000000000000, -431.3627451401119970 ) ) ;
#8843 = EDGE_CURVE ( 'NONE', #4872, #4552, #8479, .T. ) ;
#8844 =( GEOMETRIC_REPRESENTATION_CONTEXT ( 3 ) GLOBAL_UNCERTAINTY_ASSIGNED_CONTEXT ( ( #9153 ) ) GLOBAL_UNIT_ASSIGNED_CONTEXT ( ( #465, #3091, #7027 ) ) REPRESENTATION_CONTEXT ( 'NONE', 'WORKASPACE' ) );
#8845 = CARTESIAN_POINT ( 'NONE',  ( 0.1642067852079997503, 12.59486910148998895, -302.9207377450070453 ) ) ;
#8846 = CARTESIAN_POINT ( 'NONE',  ( -3.204766135845001696, -12.34903855201999079, 318.8802828394900644 ) ) ;
#8847 = ORIENTED_EDGE ( 'NONE', *, *, #8771, .T. ) ;
#8848 = CARTESIAN_POINT ( 'NONE',  ( 11.96281778373999849, -6.662668310474999522, -315.0848619657999734 ) ) ;
#8849 = EDGE_CURVE ( 'NONE', #1205, #4813, #5557, .T. ) ;
#8850 = CARTESIAN_POINT ( 'NONE',  ( -38.38033378105252780, -2.500000000000000000, -506.9690816445435644 ) ) ;
#8851 = ORIENTED_EDGE ( 'NONE', *, *, #9204, .T. ) ;
#8852 = CARTESIAN_POINT ( 'NONE',  ( -15.60615175339998473, -6.374933892835006333, 190.0071920248299477 ) ) ;
#8853 = CARTESIAN_POINT ( 'NONE',  ( 17.64879272652970599, 5.897502810282468921, 190.9999999999996589 ) ) ;
#8854 = DIRECTION ( 'NONE',  ( -0.4716280258120416069, 0.000000000000000000, 0.8817975988108813779 ) ) ;
#8855 = AXIS2_PLACEMENT_3D ( 'NONE', #9226, #9416, #5072 ) ;
#8856 = CARTESIAN_POINT ( 'NONE',  ( -16.54291557298000370, -1.991497705781999805, 315.0848619657999734 ) ) ;
#8857 = CARTESIAN_POINT ( 'NONE',  ( 10.79636471171000167, 9.449795599854001082, 320.0000000000000000 ) ) ;
#8858 = CARTESIAN_POINT ( 'NONE',  ( 9.539154743984001428, -9.809959732869000248, 319.9928079742500131 ) ) ;
#8859 = CARTESIAN_POINT ( 'NONE',  ( -19.49702808861183101, 2.833672667318400507, 319.0000000000005116 ) ) ;
#8860 = CARTESIAN_POINT ( 'NONE',  ( -14.90555606507826170, -4.246020682187605644, -438.7487226161961189 ) ) ;
#8861 = CARTESIAN_POINT ( 'NONE',  ( -24.37035621709999944, -7.500000000000000888, -411.9118794995000030 ) ) ;
#8862 = ORIENTED_EDGE ( 'NONE', *, *, #1682, .F. ) ;
#8863 = DIRECTION ( 'NONE',  ( -0.1071946444232954182, 0.000000000000000000, 0.9942380540931651245 ) ) ;
#8864 = EDGE_CURVE ( 'NONE', #9639, #10018, #4880, .T. ) ;
#8865 = CARTESIAN_POINT ( 'NONE',  ( -17.68025656702000603, 5.978840677964003092, 190.4207385301700128 ) ) ;
#8866 = DIRECTION ( 'NONE',  ( 0.000000000000000000, -1.000000000000000000, 0.000000000000000000 ) ) ;
#8867 = B_SPLINE_CURVE_WITH_KNOTS ( 'NONE', 3,
 ( #8371, #9244, #5145, #212, #4347, #7620, #9988, #955, #106, #1007, #3543, #7463, #4295, #4242, #10094, #6822, #3490, #2734, #3383, #2630, #6658, #156 ),
 .UNSPECIFIED., .F., .F.,
 ( 4, 2, 2, 2, 2, 2, 2, 2, 2, 2, 4 ),
 ( 0.4999983561373720353, 0.5624985616202005101, 0.5937486643616147752, 0.6249987671030289293, 0.6562488698444431945, 0.6874989725858574596, 0.7499991780686858789, 0.8124993835515144092, 0.8749995890343429394, 0.9374997945171714697, 1.000000000000000000 ),
 .UNSPECIFIED. ) ;
#8868 = ORIENTED_EDGE ( 'NONE', *, *, #3844, .T. ) ;
#8869 = CARTESIAN_POINT ( 'NONE',  ( 11.71572875766478639, -12.49999999885353041, -303.4999999999999432 ) ) ;
#8870 = CARTESIAN_POINT ( 'NONE',  ( 15.47214269673303200, 3.911151857093433382, 315.0000000000000568 ) ) ;
#8871 = DIRECTION ( 'NONE',  ( 1.000000000000000000, 0.000000000000000000, 0.000000000000000000 ) ) ;
#8872 = CARTESIAN_POINT ( 'NONE',  ( 17.13182678275000370, -0.2945984483948000388, -314.8616023057000461 ) ) ;
#8873 = SURFACE_STYLE_FILL_AREA ( #2377 ) ;
#8874 = CARTESIAN_POINT ( 'NONE',  ( -18.32873049326003212, 4.258249849688001909, 320.0770942683900557 ) ) ;
#8875 = DIRECTION ( 'NONE',  ( 0.000000000000000000, 1.000000000000000000, 0.000000000000000000 ) ) ;
#8876 = CARTESIAN_POINT ( 'NONE',  ( -1.698905183273398123, -2.643595541597000942, -434.8557611820924080 ) ) ;
#8877 = ORIENTED_EDGE ( 'NONE', *, *, #4382, .F. ) ;
#8878 = CARTESIAN_POINT ( 'NONE',  ( 18.87261805073000787, -0.3452380817474001162, -317.4928077629770087 ) ) ;
#8879 = CARTESIAN_POINT ( 'NONE',  ( 8.092749801746995431, -11.43508185634000007, -316.3802825947000201 ) ) ;
#8880 = EDGE_CURVE ( 'NONE', #9600, #700, #9143, .T. ) ;
#8881 = CARTESIAN_POINT ( 'NONE',  ( -46.74071243419000155, 2.500000000000000000, -414.3237589990000629 ) ) ;
#8882 = ORIENTED_EDGE ( 'NONE', *, *, #5029, .T. ) ;
#8883 = CIRCLE ( 'NONE', #9567, 1.999999999999980238 ) ;
#8884 = DIRECTION ( 'NONE',  ( -0.9968876850330226080, 0.000000000000000000, 0.07883491250392142546 ) ) ;
#8885 = PRODUCT_DEFINITION ( 'UNKNOWN', '', #7818, #3135 ) ;
#8886 = CARTESIAN_POINT ( 'NONE',  ( -8.988119689606875795, 8.550792887852695756, -314.5455502384737656 ) ) ;
#8887 = ORIENTED_EDGE ( 'NONE', *, *, #10397, .F. ) ;
#8888 = CARTESIAN_POINT ( 'NONE',  ( -3.205490369836121900, -12.35619803902316782, 319.0000000000003979 ) ) ;
#8889 = ORIENTED_EDGE ( 'NONE', *, *, #7939, .T. ) ;
#8890 = DIRECTION ( 'NONE',  ( 0.000000000000000000, 1.000000000000000000, -0.000000000000000000 ) ) ;
#8891 = EDGE_LOOP ( 'NONE', ( #1719, #1750, #7173, #4201 ) ) ;
#8892 = CARTESIAN_POINT ( 'NONE',  ( -3.023938872602656591, -9.348098599112928397, 315.0000000000000568 ) ) ;
#8893 = CARTESIAN_POINT ( 'NONE',  ( 18.93783568409002172, -3.175510411809001177, -302.4229045757450081 ) ) ;
#8894 = CARTESIAN_POINT ( 'NONE',  ( -2.000000000000000000, -9.500000000000000000, -414.5000000000000000 ) ) ;
#8895 = CARTESIAN_POINT ( 'NONE',  ( 28.53863984632670636, -2.500000000000000000, -506.8274460463252353 ) ) ;
#8896 = ADVANCED_FACE ( 'NONE', ( #6015, #8487 ), #3503, .T. ) ;
#8897 = CARTESIAN_POINT ( 'NONE',  ( 1.957937398543000418, 12.03510449230999768, -302.4229045757450081 ) ) ;
#8898 = CARTESIAN_POINT ( 'NONE',  ( -72.90663470102438737, -12.50000000000000000, -371.7168990826883714 ) ) ;
#8899 = VERTEX_POINT ( 'NONE', #1781 ) ;
#8900 = CARTESIAN_POINT ( 'NONE',  ( -15.39920013370999996, -4.579805981517999669, -314.6383426456000052 ) ) ;
#8901 = CARTESIAN_POINT ( 'NONE',  ( -11.30134585255874313, -3.136348707664786239, -437.5214317848546557 ) ) ;
#8902 = ORIENTED_EDGE ( 'NONE', *, *, #9999, .F. ) ;
#8903 = CARTESIAN_POINT ( 'NONE',  ( -12.48652197162000554, -8.514177154860004038, 190.0071920248299477 ) ) ;
#8904 = CARTESIAN_POINT ( 'NONE',  ( 2.649465170252891522, 12.40913386102118388, 190.9999999999996589 ) ) ;
#8905 = DIRECTION ( 'NONE',  ( 0.000000000000000000, 1.000000000000000000, -0.000000000000000000 ) ) ;
#8906 = EDGE_CURVE ( 'NONE', #8235, #4938, #5051, .T. ) ;
#8907 = CARTESIAN_POINT ( 'NONE',  ( -17.59334121105999671, -0.04733121045982000008, 314.4150829855000211 ) ) ;
#8908 = EDGE_CURVE ( 'NONE', #269, #7707, #251, .T. ) ;
#8909 = DIRECTION ( 'NONE',  ( 0.000000000000000000, -1.000000000000000000, 0.000000000000000000 ) ) ;
#8910 = CARTESIAN_POINT ( 'NONE',  ( 7.221770056846003705, -10.51477558267000667, 319.9928079742500131 ) ) ;
#8911 = CARTESIAN_POINT ( 'NONE',  ( 18.21047658595730212, 5.188723016677323940, 319.0000000000005116 ) ) ;
#8912 = CARTESIAN_POINT ( 'NONE',  ( -10.23467949917771591, -9.999999999493891067, -302.5000000000002274 ) ) ;
#8913 = VERTEX_POINT ( 'NONE', #5966 ) ;
#8914 = DIRECTION ( 'NONE',  ( -0.9712267471052600243, 4.782300904073985984E-08, -0.2381566831044907573 ) ) ;
#8915 = AXIS2_PLACEMENT_3D ( 'NONE', #3512, #5169, #6794 ) ;
#8916 = CARTESIAN_POINT ( 'NONE',  ( -9.011282031845993856, 11.16162715973000097, 191.1197171614399792 ) ) ;
#8917 = MANIFOLD_SOLID_BREP ( 'Stock-MAS-686-1', #5382 ) ;
#8918 = CARTESIAN_POINT ( 'NONE',  ( -46.74071243419621169, -7.500000000000000888, -414.3237589990241077 ) ) ;
#8919 = CIRCLE ( 'NONE', #346, 0.5000000000000004441 ) ;
#8920 = CARTESIAN_POINT ( 'NONE',  ( -8.586595388443328147, -7.656480000000000175, -526.6836397678595176 ) ) ;
#8921 = EDGE_CURVE ( 'NONE', #6648, #10492, #10105, .T. ) ;
#8922 = APPLICATION_PROTOCOL_DEFINITION ( 'draft international standard', 'automotive_design', 1998, #7443 ) ;
#8923 = CARTESIAN_POINT ( 'NONE',  ( 14.97723399828063506, -8.302382553459793257, -303.4999999999996589 ) ) ;
#8924 = CARTESIAN_POINT ( 'NONE',  ( -14.32653628403999946, -7.536184728883000616, -302.5000000000000000 ) ) ;
#8925 = LINE ( 'NONE', #9626, #7219 ) ;
#8926 = CARTESIAN_POINT ( 'NONE',  ( -46.36553117871467578, -7.500000000000000888, -417.8035921883502510 ) ) ;
#8927 = CARTESIAN_POINT ( 'NONE',  ( -6.055260875802999543, 12.00648505189998971, 319.5792614743400009 ) ) ;
#8928 = DIRECTION ( 'NONE',  ( -0.4712473909295803454, 0.000000000000000000, 0.8820010751365688906 ) ) ;
#8929 = CARTESIAN_POINT ( 'NONE',  ( 15.00000000000071587, 0.4945770392355663403, 315.0000000000001705 ) ) ;
#8930 = ORIENTED_EDGE ( 'NONE', *, *, #6824, .T. ) ;
#8931 = CARTESIAN_POINT ( 'NONE',  ( 18.53690224725999514, 4.739426065905003149, -316.3802825947000201 ) ) ;
#8932 = CIRCLE ( 'NONE', #7367, 3.999999999999996447 ) ;
#8933 = DIRECTION ( 'NONE',  ( 0.000000000000000000, -1.000000000000000000, 0.000000000000000000 ) ) ;
#8934 = EDGE_LOOP ( 'NONE', ( #5365, #7136, #4648, #3863 ) ) ;
#8935 = FACE_OUTER_BOUND ( 'NONE', #10511, .T. ) ;
#8936 = CARTESIAN_POINT ( 'NONE',  ( -1.713290296832884474, -7.307229827337997641, -435.0847711425938087 ) ) ;
#8937 = MANIFOLD_SOLID_BREP ( 'Stock-MAS-686-1', #1450 ) ;
#8938 = CARTESIAN_POINT ( 'NONE',  ( -72.90663470102438737, -12.40000000000001101, -371.7168990826883714 ) ) ;
#8939 = CARTESIAN_POINT ( 'NONE',  ( -9.847343584659236981, 8.231878686604520823, -314.5529121822860361 ) ) ;
#8940 = ORIENTED_EDGE ( 'NONE', *, *, #5141, .T. ) ;
#8941 = CARTESIAN_POINT ( 'NONE',  ( 8.773569371117815763, -11.24325377545516602, 319.0000000000003979 ) ) ;
#8942 = EDGE_LOOP ( 'NONE', ( #5657, #4255, #10442, #5723 ) ) ;
#8943 = DIRECTION ( 'NONE',  ( 0.000000000000000000, -1.000000000000000000, 0.000000000000000000 ) ) ;
#8944 = EDGE_LOOP ( 'NONE', ( #4060, #10020, #3663, #7623, #9656, #8458 ) ) ;
#8945 = CARTESIAN_POINT ( 'NONE',  ( -8.666088325696231109, -8.161304309888411268, 315.0000000000000568 ) ) ;
#8946 = CARTESIAN_POINT ( 'NONE',  ( 18.56223039349998771, -4.700611568415998143, -303.6197174156509391 ) ) ;
#8947 = DIRECTION ( 'NONE',  ( 0.9712267471052594692, 0.000000000000000000, 0.2381566831044984456 ) ) ;
#8948 = CARTESIAN_POINT ( 'NONE',  ( -1.873948611771682149, -7.500000000000000888, -349.2478646809681777 ) ) ;
#8949 = ORIENTED_EDGE ( 'NONE', *, *, #8908, .F. ) ;
#8950 = ADVANCED_FACE ( 'NONE', ( #7838 ), #173, .T. ) ;
#8951 = CARTESIAN_POINT ( 'NONE',  ( -19.46926817186999514, 1.611439533454998241, -302.4229045757450081 ) ) ;
#8952 = CARTESIAN_POINT ( 'NONE',  ( -59.08872748607741698, -2.500000000000000000, -420.9212224720619702 ) ) ;
#8953 = ORIENTED_EDGE ( 'NONE', *, *, #693, .F. ) ;
#8954 = CARTESIAN_POINT ( 'NONE',  ( 13.50042001888999899, -6.225262767767000049, -314.6383426456000052 ) ) ;
#8955 = CARTESIAN_POINT ( 'NONE',  ( 15.26659686508999947, 6.829480052022000258, -302.5000000000000000 ) ) ;
#8956 = EDGE_LOOP ( 'NONE', ( #8153, #8424, #9336, #9911, #5604, #160 ) ) ;
#8957 = VECTOR ( 'NONE', #10004, 1000.000000000000000 ) ;
#8958 = CARTESIAN_POINT ( 'NONE',  ( 3.087789584922997932, -11.94493704178999671, 189.9229057364800042 ) ) ;
#8959 = CARTESIAN_POINT ( 'NONE',  ( -7.895350322657909814, -8.000000000000000000, -398.4775300148394308 ) ) ;
#8960 = CARTESIAN_POINT ( 'NONE',  ( 3.970004819630974957, 9.235895690467337715, -315.0000000000000568 ) ) ;
#8961 = DIRECTION ( 'NONE',  ( 0.000000000000000000, -1.000000000000000000, 0.000000000000000000 ) ) ;
#8962 = EDGE_CURVE ( 'NONE', #8821, #3465, #1098, .T. ) ;
#8963 = EDGE_CURVE ( 'NONE', #5389, #1717, #6069, .T. ) ;
#8964 = B_SPLINE_CURVE_WITH_KNOTS ( 'NONE', 3,
 ( #5419, #7843, #9460, #4622, #7953, #8695, #1452, #2155, #4737, #9514, #7894, #490, #2100, #3115, #5475, #7152, #10473, #3816, #7102, #10369, #3010, #6333 ),
 .UNSPECIFIED., .F., .F.,
 ( 4, 2, 2, 2, 2, 2, 2, 2, 2, 2, 4 ),
 ( 0.000000000000000000, 0.06249979451717146278, 0.1249995890343429256, 0.1874993835515144092, 0.2499991780686858511, 0.3124989725858572931, 0.3437488698444430835, 0.3749987671030288738, 0.4062486643616146642, 0.4374985616202004546, 0.4999983561373720353 ),
 .UNSPECIFIED. ) ;
#8965 = CARTESIAN_POINT ( 'NONE',  ( -1.285290206351000108, -10.09749793447999977, 314.4150829855000211 ) ) ;
#8966 = DIRECTION ( 'NONE',  ( 0.000000000000000000, 0.000000000000000000, 1.000000000000000000 ) ) ;
#8967 = CARTESIAN_POINT ( 'NONE',  ( 8.770005493155000664, 10.19600538561000036, 320.0000000000000000 ) ) ;
#8968 = CIRCLE ( 'NONE', #6049, 4.000000000000000000 ) ;
#8969 = CARTESIAN_POINT ( 'NONE',  ( -18.70127769336001222, -1.615776359209001312, 319.9928079742500131 ) ) ;
#8970 = CARTESIAN_POINT ( 'NONE',  ( -8.773569371117819315, 11.24325377545516780, 319.0000000000005116 ) ) ;
#8971 = FILL_AREA_STYLE_COLOUR ( '', #5048 ) ;
#8972 = DIRECTION ( 'NONE',  ( -0.1071946444232961260, 0.000000000000000000, 0.9942380540931650135 ) ) ;
#8973 = ORIENTED_EDGE ( 'NONE', *, *, #10074, .F. ) ;
#8974 = CARTESIAN_POINT ( 'NONE',  ( 14.79012398733999945, 1.483731117707000058, -285.0000000000000000 ) ) ;
#8975 = ORIENTED_EDGE ( 'NONE', *, *, #1774, .F. ) ;
#8976 = AXIS2_PLACEMENT_3D ( 'NONE', #6246, #5438, #7973 ) ;
#8977 = MANIFOLD_SOLID_BREP ( 'Stock-MAS-686-1', #9865 ) ;
#8978 = ORIENTED_EDGE ( 'NONE', *, *, #363, .F. ) ;
#8979 = DIRECTION ( 'NONE',  ( 0.000000000000000000, 1.000000000000000000, 0.000000000000000000 ) ) ;
#8980 = CYLINDRICAL_SURFACE ( 'NONE', #6211, 12.50000000000002487 ) ;
#8981 = CONTEXT_DEPENDENT_SHAPE_REPRESENTATION ( #4353, #3902 ) ;
#8982 = CARTESIAN_POINT ( 'NONE',  ( -15.92130416703352935, -7.586839038430808202, -303.4999999999996589 ) ) ;
#8983 = CARTESIAN_POINT ( 'NONE',  ( 17.42228208267999889, 1.444224815522999972, -314.4150829855000211 ) ) ;
#8984 = CARTESIAN_POINT ( 'NONE',  ( -34.37192209818999800, -2.500000000000000000, -461.0868123482000556 ) ) ;
#8985 = CARTESIAN_POINT ( 'NONE',  ( -3.554202447527484487, -7.055426064859528168, -436.0573967677022438 ) ) ;
#8986 = CARTESIAN_POINT ( 'NONE',  ( 14.04143820182998503, 8.903536631273988533, 318.8802828394900644 ) ) ;
#8987 = DIRECTION ( 'NONE',  ( 0.1736481776669025201, 0.000000000000000000, -0.9848077530122130163 ) ) ;
#8988 = CARTESIAN_POINT ( 'NONE',  ( -7.006889269069000115, 6.844138725329000472, 315.0000000000001705 ) ) ;
#8989 = DIRECTION ( 'NONE',  ( 0.000000000000000000, -1.000000000000000000, 0.000000000000000000 ) ) ;
#8990 = CARTESIAN_POINT ( 'NONE',  ( -11.75551710966999153, 10.11738730586000123, -316.3802825947000201 ) ) ;
#8991 = LINE ( 'NONE', #5757, #1539 ) ;
#8992 = DIRECTION ( 'NONE',  ( 0.000000000000000000, -1.000000000000000000, 0.000000000000000000 ) ) ;
#8993 = ORIENTED_EDGE ( 'NONE', *, *, #9101, .F. ) ;
#8994 = CARTESIAN_POINT ( 'NONE',  ( -0.2029048030085919552, -7.657414115644002983, -433.8324684254904469 ) ) ;
#8995 = CARTESIAN_POINT ( 'NONE',  ( -3.339933055294987074, -9.500000000000001776, -397.0720243238112630 ) ) ;
#8996 = CARTESIAN_POINT ( 'NONE',  ( 14.21145943247442744, -5.188748475648757186, -315.0000000000000000 ) ) ;
#8997 = ORIENTED_EDGE ( 'NONE', *, *, #6986, .F. ) ;
#8998 = CARTESIAN_POINT ( 'NONE',  ( -2.000000000003786749, -8.000000000000000000, -409.4999999999758415 ) ) ;
#8999 = PRESENTATION_LAYER_ASSIGNMENT (  '', '', ( #8640 ) ) ;
#9000 = ORIENTED_EDGE ( 'NONE', *, *, #6063, .T. ) ;
#9001 = CARTESIAN_POINT ( 'NONE',  ( -0.6596894340221253206, -7.499999891561000886, -434.1397621899948263 ) ) ;
#9002 = EDGE_LOOP ( 'NONE', ( #7494, #1479 ) ) ;
#9003 = CARTESIAN_POINT ( 'NONE',  ( 13.97988708520999701, -9.045087908074000538, -302.9207377450070453 ) ) ;
#9004 = CARTESIAN_POINT ( 'NONE',  ( -43.46674421124934184, -8.000000000000000000, -402.7790142173016648 ) ) ;
#9005 = FACE_OUTER_BOUND ( 'NONE', #2661, .T. ) ;
#9006 = APPLICATION_CONTEXT ( 'automotive_design' ) ;
#9007 = VECTOR ( 'NONE', #1221, 1000.000000000000000 ) ;
#9008 = AXIS2_PLACEMENT_3D ( 'NONE', #3573, #10176, #5126 ) ;
#9009 = AXIS2_PLACEMENT_3D ( 'NONE', #1077, #5363, #6789 ) ;
#9010 = CARTESIAN_POINT ( 'NONE',  ( -2.272374192480355326, -7.400653393618207510, -434.9211848868894208 ) ) ;
#9011 = CARTESIAN_POINT ( 'NONE',  ( -10.25126250535807770, -10.00000007971003058, 314.4997059534069308 ) ) ;
#9012 = VERTEX_POINT ( 'NONE', #6937 ) ;
#9013 = CARTESIAN_POINT ( 'NONE',  ( -16.98808798087999961, -1.334629195702000004, -314.8616023057000461 ) ) ;
#9014 = DIRECTION ( 'NONE',  ( 0.000000000000000000, -1.000000000000000000, 0.000000000000000000 ) ) ;
#9015 = ORIENTED_EDGE ( 'NONE', *, *, #6253, .F. ) ;
#9016 = CARTESIAN_POINT ( 'NONE',  ( -13.05089818882000507, -9.570190452814999915, 190.4207385301700128 ) ) ;
#9017 = DIRECTION ( 'NONE',  ( -0.4712473909295827323, 0.000000000000000000, 0.8820010751365675583 ) ) ;
#9018 = CARTESIAN_POINT ( 'NONE',  ( 15.26192592288500194, 4.160213195839838285, -315.0000000000000000 ) ) ;
#9019 = CARTESIAN_POINT ( 'NONE',  ( -8.518317708839887814, -7.500000000000000000, -528.6824739677025491 ) ) ;
#9020 = CARTESIAN_POINT ( 'NONE',  ( 15.92197846796999983, -3.582977715798000062, 314.8616023057000461 ) ) ;
#9021 =( LENGTH_UNIT ( ) NAMED_UNIT ( * ) SI_UNIT ( .MILLI., .METRE. ) );
#9022 = CARTESIAN_POINT ( 'NONE',  ( 4.804283134583999804, 11.13634285072000019, 320.0000000000000000 ) ) ;
#9023 = CARTESIAN_POINT ( 'NONE',  ( 17.27957593929000879, -4.562754682971998932, 319.9928079742500131 ) ) ;
#9024 = CARTESIAN_POINT ( 'NONE',  ( -0.6338995735901450379, 12.51432109910910029, 319.0000000000005116 ) ) ;
#9025 = SURFACE_STYLE_USAGE ( .BOTH. , #9190 ) ;
#9026 = CARTESIAN_POINT ( 'NONE',  ( -73.93978370014021095, -12.50000000000000000, -368.3728591389038911 ) ) ;
#9027 = ORIENTED_EDGE ( 'NONE', *, *, #5385, .F. ) ;
#9028 = DIRECTION ( 'NONE',  ( 0.3420201433256988555, 0.000000000000000000, -0.9396926207858975477 ) ) ;
#9029 = ORIENTED_EDGE ( 'NONE', *, *, #1752, .F. ) ;
#9030 = DIRECTION ( 'NONE',  ( 3.267118270366935116E-06, 8.358028861085000358E-13, -0.9999999999946629359 ) ) ;
#9031 = CIRCLE ( 'NONE', #5988, 3.500000000000003109 ) ;
#9032 = CARTESIAN_POINT ( 'NONE',  ( 15.75886148104574325, 3.542954957252464343, 315.0000000000000000 ) ) ;
#9033 = LINE ( 'NONE', #709, #6688 ) ;
#9034 = CARTESIAN_POINT ( 'NONE',  ( 16.92248268936999978, 0.04189409840125999512, -315.0848619657999734 ) ) ;
#9035 = EDGE_CURVE ( 'NONE', #9273, #3853, #9038, .T. ) ;
#9036 = FILL_AREA_STYLE_COLOUR ( '', #1198 ) ;
#9037 = CARTESIAN_POINT ( 'NONE',  ( -1.832041979401632714, -7.303110144047968433, -435.2805036650163970 ) ) ;
#9038 = B_SPLINE_CURVE_WITH_KNOTS ( 'NONE', 3,
 ( #7890, #7045, #5311, #10364 ),
 .UNSPECIFIED., .F., .F.,
 ( 4, 4 ),
 ( 0.000000000000000000, 1.000000000000000000 ),
 .UNSPECIFIED. ) ;
#9039 = CARTESIAN_POINT ( 'NONE',  ( -14.95234154667176973, -5.997675161540820810, -438.5579267480833323 ) ) ;
#9040 = EDGE_CURVE ( 'NONE', #6576, #3582, #537, .T. ) ;
#9041 = CARTESIAN_POINT ( 'NONE',  ( 11.28781796570999951, 4.951468039558000633, -284.9999999999999432 ) ) ;
#9042 = LINE ( 'NONE', #177, #5218 ) ;
#9043 = ADVANCED_BREP_SHAPE_REPRESENTATION ( '', ( #1856, #2817 ), #6445 ) ;
#9044 = CARTESIAN_POINT ( 'NONE',  ( -18.56065892533998962, 4.703159488203003669, -316.3802825947000201 ) ) ;
#9045 = VERTEX_POINT ( 'NONE', #4673 ) ;
#9046 = CARTESIAN_POINT ( 'NONE',  ( -18.99997784094000153, -0.3131176371119000490, 319.9999999999899956 ) ) ;
#9047 = EDGE_CURVE ( 'NONE', #7746, #886, #1621, .T. ) ;
#9048 = CARTESIAN_POINT ( 'NONE',  ( -1.652955156006773230, -7.314598583700001377, -435.0632706482025469 ) ) ;
#9049 = DIRECTION ( 'NONE',  ( 0.000000000000000000, -1.000000000000000000, 0.000000000000000000 ) ) ;
#9050 = CARTESIAN_POINT ( 'NONE',  ( 8.691431531408321476, -8.152829611300951740, -315.0000000000000000 ) ) ;
#9051 = ORIENTED_EDGE ( 'NONE', *, *, #5619, .T. ) ;
#9052 = DIRECTION ( 'NONE',  ( 0.000000000000000000, 1.000000000000000000, -0.000000000000000000 ) ) ;
#9053 = ORIENTED_EDGE ( 'NONE', *, *, #9566, .F. ) ;
#9054 = CARTESIAN_POINT ( 'NONE',  ( 16.89340345063000015, 5.253727359668999952, -317.4999999999989768 ) ) ;
#9055 = ORIENTED_EDGE ( 'NONE', *, *, #6395, .T. ) ;
#9056 = CARTESIAN_POINT ( 'NONE',  ( 17.80660862177001746, -5.847896592537999538, -302.9207377450070453 ) ) ;
#9057 = CARTESIAN_POINT ( 'NONE',  ( 6.508337484872001255, -10.68452134396000375, -317.4928077629770087 ) ) ;
#9058 = DIRECTION ( 'NONE',  ( -0.2951854283188049544, 0.000000000000000000, 0.9554399839384174475 ) ) ;
#9059 = AXIS2_PLACEMENT_3D ( 'NONE', #492, #7955, #5422 ) ;
#9060 =( LENGTH_UNIT ( ) NAMED_UNIT ( * ) SI_UNIT ( .MILLI., .METRE. ) );
#9061 = CARTESIAN_POINT ( 'NONE',  ( -20.10149561490999659, 0.3453761138107002138, -302.9207377450070453 ) ) ;
#9062 = EDGE_CURVE ( 'NONE', #5121, #3477, #1229, .T. ) ;
#9063 = DIRECTION ( 'NONE',  ( 0.000000000000000000, -1.000000000000000000, 0.000000000000000000 ) ) ;
#9064 = ORIENTED_EDGE ( 'NONE', *, *, #30, .T. ) ;
#9065 = CARTESIAN_POINT ( 'NONE',  ( -13.22841524816015202, -3.249999927714000147, -437.9939944912570127 ) ) ;
#9066 = DIRECTION ( 'NONE',  ( 0.000000000000000000, -1.000000000000000000, 0.000000000000000000 ) ) ;
#9067 = VERTEX_POINT ( 'NONE', #486 ) ;
#9068 = CARTESIAN_POINT ( 'NONE',  ( -19.21810730420998681, -3.675731523933000400, 190.4207385301700128 ) ) ;
#9069 = AXIS2_PLACEMENT_3D ( 'NONE', #3511, #283, #5219 ) ;
#9070 = CARTESIAN_POINT ( 'NONE',  ( 8.037373804805000077, -9.179324345868998591, -315.0000000000001137 ) ) ;
#9071 = CARTESIAN_POINT ( 'NONE',  ( 15.44329739658677880, 3.946306641738668297, -314.9999999999999432 ) ) ;
#9072 = CARTESIAN_POINT ( 'NONE',  ( -2.000000000003786749, -7.500000000000000888, -409.4999999999758415 ) ) ;
#9073 = CARTESIAN_POINT ( 'NONE',  ( 17.34693632642999717, 0.4167404706239999923, 314.6383426456000052 ) ) ;
#9074 =( NAMED_UNIT ( * ) PLANE_ANGLE_UNIT ( ) SI_UNIT ( $, .RADIAN. ) );
#9075 = FACE_OUTER_BOUND ( 'NONE', #5323, .T. ) ;
#9076 = CARTESIAN_POINT ( 'NONE',  ( 19.10207382662997588, -2.686351016941002534, 320.0770942683900557 ) ) ;
#9077 = CARTESIAN_POINT ( 'NONE',  ( -10.97430844189483778, 10.45950866754415820, 319.0000000000005116 ) ) ;
#9078 = CARTESIAN_POINT ( 'NONE',  ( 3.693615097834042960, 12.29963531854552450, -303.5000000000000000 ) ) ;
#9079 = CARTESIAN_POINT ( 'NONE',  ( 17.56330558013000243, 0.6698376231023999150, 314.4150829855000211 ) ) ;
#9080 = ORIENTED_EDGE ( 'NONE', *, *, #7471, .F. ) ;
#9081 = LINE ( 'NONE', #3547, #6378 ) ;
#9082 = ORIENTED_EDGE ( 'NONE', *, *, #7851, .F. ) ;
#9083 = EDGE_LOOP ( 'NONE', ( #4629, #4298, #2974, #2166 ) ) ;
#9084 = CARTESIAN_POINT ( 'NONE',  ( -1.761667614806367244, -2.511152837933000370, -434.6216513933122769 ) ) ;
#9085 =( BOUNDED_SURFACE ( )  B_SPLINE_SURFACE ( 3, 1, ( 
 ( #3709, #1230 ),
 ( #4508, #7786 ),
 ( #1337, #431 ),
 ( #4616, #6993 ),
 ( #2096, #749 ),
 ( #8215, #5740 ),
 ( #4030, #1448 ) ),
 .UNSPECIFIED., .F., .F., .T. ) 
 B_SPLINE_SURFACE_WITH_KNOTS ( ( 4, 3, 4 ),
 ( 2, 2 ),
 ( 0.000000000000000000, 0.5000000000000000000, 1.000000000000000000 ),
 ( 0.000000000000000000, 1.000000000000000000 ),
 .UNSPECIFIED. ) 
 GEOMETRIC_REPRESENTATION_ITEM ( )  RATIONAL_B_SPLINE_SURFACE ( (
 ( 1.000000000000000000, 1.000000000000000000),
 ( 0.8047378540805999458, 0.8047378540805999458),
 ( 0.8047378540805999458, 0.8047378540805999458),
 ( 1.000000000000000000, 1.000000000000000000),
 ( 0.8047378540805999458, 0.8047378540805999458),
 ( 0.8047378540805999458, 0.8047378540805999458),
 ( 1.000000000000000000, 1.000000000000000000) ) ) 
 REPRESENTATION_ITEM ( '' )  SURFACE ( )  );
#9086 = CARTESIAN_POINT ( 'NONE',  ( 3.023938872602656591, 9.348098599112928397, 315.0000000000000568 ) ) ;
#9087 = ITEM_DEFINED_TRANSFORMATION ( 'NONE', 'NONE', #6975,  #2817 ) ;
#9088 = CARTESIAN_POINT ( 'NONE',  ( -101.0297452788102817, -7.500000000000000000, -342.4231267849074811 ) ) ;
#9089 = ORIENTED_EDGE ( 'NONE', *, *, #3710, .T. ) ;
#9090 = AXIS2_PLACEMENT_3D ( 'NONE', #3293, #7330, #1582 ) ;
#9091 = CARTESIAN_POINT ( 'NONE',  ( -1.073657119321965059, -2.527164246181165197, -434.4475771139335052 ) ) ;
#9092 = VECTOR ( 'NONE', #9850, 1000.000000000000227 ) ;
#9093 = EDGE_CURVE ( 'NONE', #6915, #10437, #4367, .T. ) ;
#9094 = DIRECTION ( 'NONE',  ( 0.000000000000000000, 1.000000000000000000, 0.000000000000000000 ) ) ;
#9095 = CARTESIAN_POINT ( 'NONE',  ( -0.3336219746636178707, -2.411421344994997717, -434.6316404192452865 ) ) ;
#9096 = CARTESIAN_POINT ( 'NONE',  ( -46.74071243416547361, -7.500000000000000000, -414.3237589990478114 ) ) ;
#9097 = CARTESIAN_POINT ( 'NONE',  ( -5.321980890543003717, 12.05475797716000486, -316.3802825947000201 ) ) ;
#9098 = VECTOR ( 'NONE', #483, 1000.000000000000000 ) ;
#9099 = ADVANCED_FACE ( 'NONE', ( #10314 ), #1336, .F. ) ;
#9100 = CARTESIAN_POINT ( 'NONE',  ( 6.710635551220206274, -4.448381107550146929, -525.2761360244785465 ) ) ;
#9101 = EDGE_CURVE ( 'NONE', #3094, #4107, #592, .T. ) ;
#9102 = CARTESIAN_POINT ( 'NONE',  ( -0.3470087687485771677, -7.585217605017000153, -434.6423010044687203 ) ) ;
#9103 = DIRECTION ( 'NONE',  ( -5.580921738635028310E-06, 2.007400790903078554E-12, 0.9999999999844266796 ) ) ;
#9104 = CARTESIAN_POINT ( 'NONE',  ( 15.60727917143683108, -3.742131089528405674, -315.0000000000000000 ) ) ;
#9105 = VERTEX_POINT ( 'NONE', #2094 ) ;
#9106 = AXIS2_PLACEMENT_3D ( 'NONE', #8223, #5590, #7422 ) ;
#9107 = CARTESIAN_POINT ( 'NONE',  ( 3.644504295958670426, -9.783030308347003157, -314.5117835914682018 ) ) ;
#9108 = ORIENTED_EDGE ( 'NONE', *, *, #7077, .F. ) ;
#9109 = DIRECTION ( 'NONE',  ( -0.6156614753245235327, 0.000000000000000000, 0.7880107536076085273 ) ) ;
#9110 = ORIENTED_EDGE ( 'NONE', *, *, #2451, .F. ) ;
#9111 = CARTESIAN_POINT ( 'NONE',  ( -19.86714287764001696, -1.744094218545000352, -303.6197174156509391 ) ) ;
#9112 = CARTESIAN_POINT ( 'NONE',  ( -7.576881921353003868, -10.42269368856000611, -317.4928077629770087 ) ) ;
#9113 = ADVANCED_FACE ( 'NONE', ( #5415 ), #5360, .T. ) ;
#9114 = CARTESIAN_POINT ( 'NONE',  ( -10.00000000000000000, -2.500000000000000000, -317.5000000000000000 ) ) ;
#9115 =( NAMED_UNIT ( * ) SI_UNIT ( $, .STERADIAN. ) SOLID_ANGLE_UNIT ( ) );
#9116 = CARTESIAN_POINT ( 'NONE',  ( -11.30134943970389827, -6.863654245155042410, -437.5214327350141730 ) ) ;
#9117 = CARTESIAN_POINT ( 'NONE',  ( 19.58578074103492739, -1.999241604668525937E-07, -302.5000071933976642 ) ) ;
#9118 = ORIENTED_EDGE ( 'NONE', *, *, #113, .T. ) ;
#9119 = CARTESIAN_POINT ( 'NONE',  ( -16.19514236092000203, -2.730451569713999938, -315.0848619657999734 ) ) ;
#9120 = CYLINDRICAL_SURFACE ( 'NONE', #1804, 5.000000000000008882 ) ;
#9121 = ORIENTED_EDGE ( 'NONE', *, *, #5938, .T. ) ;
#9122 = CARTESIAN_POINT ( 'NONE',  ( 17.68025656702000603, -5.978840677964003092, 190.4207385301700128 ) ) ;
#9123 = CARTESIAN_POINT ( 'NONE',  ( -72.90663470102438737, -2.599999999999984102, -371.7168990826883714 ) ) ;
#9124 = CARTESIAN_POINT ( 'NONE',  ( -49.82771619714345235, -7.500000000000000000, -415.9731248673013511 ) ) ;
#9125 = DIRECTION ( 'NONE',  ( -0.8820010751365676693, 0.000000000000000000, -0.4712473909295822883 ) ) ;
#9126 = CARTESIAN_POINT ( 'NONE',  ( -14.83086724907998999, 8.388894394345001615, 191.1197171614399792 ) ) ;
#9127 = VECTOR ( 'NONE', #4898, 1000.000000000000000 ) ;
#9128 = CARTESIAN_POINT ( 'NONE',  ( 14.28417481768999941, -5.042936695466000430, 315.0848619657999734 ) ) ;
#9129 = CARTESIAN_POINT ( 'NONE',  ( -64.74703706732441333, -8.000000000000000000, -381.8372235071373666 ) ) ;
#9130 = CARTESIAN_POINT ( 'NONE',  ( 16.76867785761999485, -5.202124494729996940, 319.9928079742500131 ) ) ;
#9131 = DIRECTION ( 'NONE',  ( -0.7784864941890657919, 0.000000000000000000, -0.6276613564377031551 ) ) ;
#9132 = DIRECTION ( 'NONE',  ( -0.9942380540931649024, 0.000000000000000000, -0.1071946444232959872 ) ) ;
#9133 = CARTESIAN_POINT ( 'NONE',  ( 1.257430124576000008, 9.427442400486999219, 315.0848619657999734 ) ) ;
#9134 = EDGE_LOOP ( 'NONE', ( #9991, #4536 ) ) ;
#9135 = CARTESIAN_POINT ( 'NONE',  ( -8.835721849737739220, -11.22420793802478123, 190.9999999999995737 ) ) ;
#9136 = VERTEX_POINT ( 'NONE', #6224 ) ;
#9137 = CARTESIAN_POINT ( 'NONE',  ( -13.28926728532226242, -3.829332416735001576, -437.9231028215058359 ) ) ;
#9138 = CARTESIAN_POINT ( 'NONE',  ( -8.647614135908284538, 8.167456227882626152, 315.0000000000000568 ) ) ;
#9139 = CONTEXT_DEPENDENT_SHAPE_REPRESENTATION ( #7302, #7083 ) ;
#9140 = CARTESIAN_POINT ( 'NONE',  ( 11.28781796570999951, -4.951468039558000633, -285.0000000000000000 ) ) ;
#9141 = EDGE_LOOP ( 'NONE', ( #6377, #8624 ) ) ;
#9142 = CARTESIAN_POINT ( 'NONE',  ( -10.00000000000000000, 2.500000000000000000, -317.5000000000000000 ) ) ;
#9143 = LINE ( 'NONE', #7478, #77 ) ;
#9144 = CARTESIAN_POINT ( 'NONE',  ( -1.419234048971399931, -7.135492406320001813, -435.1303133261055223 ) ) ;
#9145 = CARTESIAN_POINT ( 'NONE',  ( -15.52898264372803006, 3.840979768096379310, -315.0000000000000000 ) ) ;
#9146 = AXIS2_PLACEMENT_3D ( 'NONE', #7706, #7658, #5183 ) ;
#9147 = CARTESIAN_POINT ( 'NONE',  ( -1.193878590405294648, -2.592889965380001716, -435.1143622073087158 ) ) ;
#9148 = CARTESIAN_POINT ( 'NONE',  ( -2.000000000000000000, -9.500000000000000000, -409.5000000000000000 ) ) ;
#9149 = CARTESIAN_POINT ( 'NONE',  ( 9.218822326027003911, 11.18653774893999220, -317.0792622552969533 ) ) ;
#9150 = ADVANCED_FACE ( 'NONE', ( #8691 ), #9688, .T. ) ;
#9151 = FACE_BOUND ( 'NONE', #7966, .T. ) ;
#9152 = CARTESIAN_POINT ( 'NONE',  ( -1.449792573629281600, -7.363504377864001249, -435.2149157260363381 ) ) ;
#9153 = UNCERTAINTY_MEASURE_WITH_UNIT (LENGTH_MEASURE( 1.000000000000000082E-05 ), #465, 'distance_accuracy_value', 'NONE');
#9154 = DIRECTION ( 'NONE',  ( 0.000000000000000000, 1.000000000000000000, -0.000000000000000000 ) ) ;
#9155 = CARTESIAN_POINT ( 'NONE',  ( 11.28358823633007901, -7.096269052248556086, -315.0000000000000568 ) ) ;
#9156 = ORIENTED_EDGE ( 'NONE', *, *, #9035, .T. ) ;
#9157 = FACE_OUTER_BOUND ( 'NONE', #8040, .T. ) ;
#9158 = VERTEX_POINT ( 'NONE', #6325 ) ;
#9159 = CARTESIAN_POINT ( 'NONE',  ( 6.294344443169999970, 10.85463315985999877, -317.5000000000000000 ) ) ;
#9160 = ORIENTED_EDGE ( 'NONE', *, *, #4000, .T. ) ;
#9161 = CARTESIAN_POINT ( 'NONE',  ( 15.96001947224000794, -7.545661119572996789, -303.6197174156509391 ) ) ;
#9162 = EDGE_CURVE ( 'NONE', #4540, #8127, #4834, .T. ) ;
#9163 = CARTESIAN_POINT ( 'NONE',  ( 19.56985579239002959, 0.3946094453810997660, -317.5770954168139610 ) ) ;
#9164 = AXIS2_PLACEMENT_3D ( 'NONE', #5463, #1279, #9504 ) ;
#9165 = CARTESIAN_POINT ( 'NONE',  ( -17.34693632642999717, -0.4167404706239999923, -314.6383426456000052 ) ) ;
#9166 = CARTESIAN_POINT ( 'NONE',  ( 0.000000000000000000, 0.000000000000000000, 0.000000000000000000 ) ) ;
#9167 = CARTESIAN_POINT ( 'NONE',  ( 20.01660392705000646, 0.3690847706228002623, -303.6197174156520759 ) ) ;
#9168 = CARTESIAN_POINT ( 'NONE',  ( -17.50000000000000000, -3.147917160613439321E-08, 315.0000000000000000 ) ) ;
#9169 =( BOUNDED_CURVE ( )  B_SPLINE_CURVE ( 3, ( #418, #2892, #7091, #3646, #4607, #1987, #5352, #6929, #2844, #4498, #3698, #6160, #7881, #10356, #7035, #9549, #2190, #8627, #1274, #2995, #4663, #10306, #6270, #5458, #475, #8736 ),
 .UNSPECIFIED., .F., .F. ) 
 B_SPLINE_CURVE_WITH_KNOTS ( ( 4, 1, 1, 1, 1, 1, 1, 1, 1, 1, 1, 1, 1, 1, 1, 1, 1, 1, 1, 1, 1, 1, 1, 4 ),
 ( 0.000000000000000000, 0.006575387376420720360, 0.03147587580142015284, 0.05343946111830009255, 0.07456689176594544222, 0.09618900060869983726, 0.1191358387887401504, 0.1441625736054258922, 0.1719175949757547894, 0.2028430032774542480, 0.2370252242332172854, 0.2743986122632974256, 0.3149466209281155393, 0.3587386281848603531, 0.4061912593601564314, 0.4578269296042451475, 0.5140479793078506221, 0.5747700779972666485, 0.6397184740335285502, 0.7086229277996399789, 0.7817513793272220513, 0.8601134552957673263, 0.9447709961445381888, 1.000000000000000000 ),
 .UNSPECIFIED. ) 
 CURVE ( )  GEOMETRIC_REPRESENTATION_ITEM ( )  RATIONAL_B_SPLINE_CURVE ( ( 1.017162749436847813, 1.017162749436847813, 1.017162749436847813, 1.017162749436847813, 1.017162749436847813, 1.017162749436847813, 1.017162749436847813, 1.017162749436847813, 1.017162749436847813, 1.017162749436847813, 1.017162749436847813, 1.017162749436847813, 1.017162749436847813, 1.017162749436847813, 1.017162749436847813, 1.017162749436847813, 1.017162749436847813, 1.017162749436847813, 1.017162749436847813, 1.017162749436847813, 1.017162749436847813, 1.017162749436847813, 1.017162749436847813, 1.017162749436847813, 1.017162749436847813, 1.017162749436847813 ) ) 
 REPRESENTATION_ITEM ( '' )  );
#9170 = ORIENTED_EDGE ( 'NONE', *, *, #7309, .F. ) ;
#9171 = CARTESIAN_POINT ( 'NONE',  ( -16.07469914181999826, -3.754035329064000059, -314.6383426456000052 ) ) ;
#9172 = EDGE_CURVE ( 'NONE', #6903, #4635, #3677, .T. ) ;
#9173 = CARTESIAN_POINT ( 'NONE',  ( -16.90628502044000214, 5.238535436438000126, -302.5000000000009663 ) ) ;
#9174 = ORIENTED_EDGE ( 'NONE', *, *, #2398, .T. ) ;
#9175 = CARTESIAN_POINT ( 'NONE',  ( 13.14174346518001535, -9.520659322650999457, 190.4207385301700128 ) ) ;
#9176 = CARTESIAN_POINT ( 'NONE',  ( 15.67978886374999803, -4.575336738469999887, -314.4944826805095772 ) ) ;
#9177 = CARTESIAN_POINT ( 'NONE',  ( -31.51838671672000558, 2.500000000000000000, -497.7560445212000104 ) ) ;
#9178 = AXIS2_PLACEMENT_3D ( 'NONE', #345, #1907, #3667 ) ;
#9179 = EDGE_CURVE ( 'NONE', #5049, #8108, #2418, .T. ) ;
#9180 = DIRECTION ( 'NONE',  ( 0.000000000000000000, -1.000000000000000000, 0.000000000000000000 ) ) ;
#9181 = CARTESIAN_POINT ( 'NONE',  ( 20.05695074155000768, -0.5616361869861998812, 190.4207385301700128 ) ) ;
#9182 = AXIS2_PLACEMENT_3D ( 'NONE', #6385, #8052, #7359 ) ;
#9183 = AXIS2_PLACEMENT_3D ( 'NONE', #10612, #4063, #2505 ) ;
#9184 = ORIENTED_EDGE ( 'NONE', *, *, #1223, .F. ) ;
#9185 = CARTESIAN_POINT ( 'NONE',  ( 16.55686070535999832, -1.955716293870999767, 315.0848619657999734 ) ) ;
#9186 = ADVANCED_FACE ( 'NONE', ( #646 ), #7147, .F. ) ;
#9187 = CARTESIAN_POINT ( 'NONE',  ( -72.90663470102438737, -2.500000000000000000, -368.3168990826883373 ) ) ;
#9188 = CARTESIAN_POINT ( 'NONE',  ( 14.12295497348999440, -7.525186449763000773, 319.9928079742500131 ) ) ;
#9189 = CARTESIAN_POINT ( 'NONE',  ( 19.00000000000000000, 0.000000000000000000, -302.5000000001010108 ) ) ;
#9190 = SURFACE_SIDE_STYLE ('',( #3384 ) ) ;
#9191 = CARTESIAN_POINT ( 'NONE',  ( 15.56325459994999960, 4.731967449628999844, 314.4150829855000211 ) ) ;
#9192 = VERTEX_POINT ( 'NONE', #10580 ) ;
#9193 = CARTESIAN_POINT ( 'NONE',  ( -46.74071243419000155, 2.500000000000000000, -414.3237589990000629 ) ) ;
#9194 = AXIS2_PLACEMENT_3D ( 'NONE', #4478, #2771, #2722 ) ;
#9195 = VECTOR ( 'NONE', #9132, 1000.000000000000114 ) ;
#9196 = ORIENTED_EDGE ( 'NONE', *, *, #7971, .F. ) ;
#9197 = CARTESIAN_POINT ( 'NONE',  ( 19.21835421908001607, 3.675208614194998447, 319.5792614743400009 ) ) ;
#9198 = CARTESIAN_POINT ( 'NONE',  ( -28.01838671672000203, 2.500000000000000000, -497.7560445212000104 ) ) ;
#9199 = CARTESIAN_POINT ( 'NONE',  ( 10.54280934634114786, 7.451587612377529091, 315.0000000000000000 ) ) ;
#9200 = CONTEXT_DEPENDENT_SHAPE_REPRESENTATION ( #7643, #5523 ) ;
#9201 = DIRECTION ( 'NONE',  ( 0.000000000000000000, -1.000000000000000000, 0.000000000000000000 ) ) ;
#9202 = EDGE_LOOP ( 'NONE', ( #9629, #2711, #8349, #10488 ) ) ;
#9203 = CARTESIAN_POINT ( 'NONE',  ( 10.14429053679999981, -9.716529139337000132, -302.5000000000000000 ) ) ;
#9204 = EDGE_CURVE ( 'NONE', #9012, #5064, #2253, .T. ) ;
#9205 = CARTESIAN_POINT ( 'NONE',  ( -13.01014152926537548, -6.185120192877000989, -437.8675655776580129 ) ) ;
#9206 = CARTESIAN_POINT ( 'NONE',  ( -76.59645255500944927, -12.50000000000000000, -359.7738992834581495 ) ) ;
#9207 = DIRECTION ( 'NONE',  ( 0.000000000000000000, 1.000000000000000000, 0.000000000000000000 ) ) ;
#9208 = EDGE_LOOP ( 'NONE', ( #5456, #3420, #4032, #7400 ) ) ;
#9209 = DIRECTION ( 'NONE',  ( 1.000000000000000000, 0.000000000000000000, 0.000000000000000000 ) ) ;
#9210 = AXIS2_PLACEMENT_3D ( 'NONE', #6753, #495, #3763 ) ;
#9211 = CYLINDRICAL_SURFACE ( 'NONE', #7168, 3.499999999999998668 ) ;
#9212 = CARTESIAN_POINT ( 'NONE',  ( -65.18634731262977766, -8.000000000000000000, -381.5491492281228716 ) ) ;
#9213 = CARTESIAN_POINT ( 'NONE',  ( -82.96626782902075092, -2.500000000000000000, -348.6449257547347997 ) ) ;
#9214 = CARTESIAN_POINT ( 'NONE',  ( 5.850354798305524184, -8.918567588720486938, -315.0000000000000000 ) ) ;
#9215 = EDGE_LOOP ( 'NONE', ( #8747, #370 ) ) ;
#9216 = CARTESIAN_POINT ( 'NONE',  ( -17.50000000000000000, 0.000000000000000000, -314.4999343908002061 ) ) ;
#9217 = CARTESIAN_POINT ( 'NONE',  ( 0.2363647329299927713, -12.51727884664821033, -316.5000000000004547 ) ) ;
#9218 = EDGE_LOOP ( 'NONE', ( #8889, #8681, #7226, #2724, #3073, #9110 ) ) ;
#9219 = CARTESIAN_POINT ( 'NONE',  ( -9.038557733644999814, 10.11114377999000169, -317.5000000000000000 ) ) ;
#9220 = ORIENTED_EDGE ( 'NONE', *, *, #1423, .F. ) ;
#9221 = CARTESIAN_POINT ( 'NONE',  ( 16.86005112630999037, 5.110605191077000065, -317.4928077629770087 ) ) ;
#9222 = AXIS2_PLACEMENT_3D ( 'NONE', #3508, #9565, #4679 ) ;
#9223 = CARTESIAN_POINT ( 'NONE',  ( -18.87261805073000787, 0.3452380817474001162, -317.4928077629770087 ) ) ;
#9224 = CARTESIAN_POINT ( 'NONE',  ( -16.99702983282000091, 1.298346578676000007, -314.8616023057000461 ) ) ;
#9225 = ORIENTED_EDGE ( 'NONE', *, *, #4000, .F. ) ;
#9226 = CARTESIAN_POINT ( 'NONE',  ( 0.000000000000000000, 0.000000000000000000, 0.000000000000000000 ) ) ;
#9227 = CARTESIAN_POINT ( 'NONE',  ( 0.1637764853584998959, 12.51053635490000282, -303.6197174156509391 ) ) ;
#9228 = CARTESIAN_POINT ( 'NONE',  ( -16.24790194983231117, -3.755744826583856000, 314.4999487198771817 ) ) ;
#9229 = ORIENTED_EDGE ( 'NONE', *, *, #7014, .T. ) ;
#9230 = CARTESIAN_POINT ( 'NONE',  ( -2.000000000000000000, 2.500000000000000000, -409.5000000000000568 ) ) ;
#9231 = CARTESIAN_POINT ( 'NONE',  ( -81.08127826530241578, -2.500000000000000000, -352.1729300552810855 ) ) ;
#9232 = ORIENTED_EDGE ( 'NONE', *, *, #7054, .T. ) ;
#9233 = CARTESIAN_POINT ( 'NONE',  ( 19.19804233804001115, -3.716674010855997690, 190.4207385301700128 ) ) ;
#9234 = DIRECTION ( 'NONE',  ( -0.8820010751365675583, 0.000000000000000000, -0.4712473909295827323 ) ) ;
#9235 = CARTESIAN_POINT ( 'NONE',  ( 15.35654050466421694, 4.050078947852131073, -315.0000000000001137 ) ) ;
#9236 = CARTESIAN_POINT ( 'NONE',  ( 19.58491037614999897, 2.818636756334000903, 190.4207385301700128 ) ) ;
#9237 = AXIS2_PLACEMENT_3D ( 'NONE', #2692, #5960, #272 ) ;
#9238 = ADVANCED_FACE ( 'NONE', ( #2470 ), #5520, .T. ) ;
#9239 = CARTESIAN_POINT ( 'NONE',  ( 15.74033075358999945, -3.452242816619000010, 315.0848619657999734 ) ) ;
#9240 =( NAMED_UNIT ( * ) PLANE_ANGLE_UNIT ( ) SI_UNIT ( $, .RADIAN. ) );
#9241 = DIRECTION ( 'NONE',  ( 0.000000000000000000, 1.000000000000000000, 0.000000000000000000 ) ) ;
#9242 = CARTESIAN_POINT ( 'NONE',  ( 14.87701781886999086, -6.977856518223995330, 319.9928079742500131 ) ) ;
#9243 = AXIS2_PLACEMENT_3D ( 'NONE', #7898, #5529, #1185 ) ;
#9244 = CARTESIAN_POINT ( 'NONE',  ( -1.604652252758985043, 9.999950698701082885, 314.4999444147077838 ) ) ;
#9245 = CARTESIAN_POINT ( 'NONE',  ( -3.427628718044569478, 12.33061748745338981, -303.4999999999990905 ) ) ;
#9246 = CARTESIAN_POINT ( 'NONE',  ( 6.322301096779000318, 8.991223814764000011, 314.8616023057000461 ) ) ;
#9247 = EDGE_LOOP ( 'NONE', ( #9835, #4581, #2454, #2829 ) ) ;
#9248 = CARTESIAN_POINT ( 'NONE',  ( -1.813125407131493949, -2.572135581867000198, -434.7536649739391237 ) ) ;
#9249 = EDGE_LOOP ( 'NONE', ( #10522, #7631, #6362, #8395 ) ) ;
#9250 = CARTESIAN_POINT ( 'NONE',  ( -16.36040776911000449, 7.306617842034003552, 319.5792614743400009 ) ) ;
#9251 = EDGE_CURVE ( 'NONE', #8913, #2473, #2870, .T. ) ;
#9252 = ADVANCED_FACE ( 'NONE', ( #9666 ), #4082, .T. ) ;
#9253 = CARTESIAN_POINT ( 'NONE',  ( -13.36185104352900055, -9.000000000000001776, -400.1641368440791098 ) ) ;
#9254 = CARTESIAN_POINT ( 'NONE',  ( 4.713955699089914297, 9.123860163919065513, 315.0000000000000568 ) ) ;
#9255 = CARTESIAN_POINT ( 'NONE',  ( 0.000000000000000000, -7.937240849781000307, -285.0000000000000000 ) ) ;
#9256 = ORIENTED_EDGE ( 'NONE', *, *, #8297, .F. ) ;
#9257 = DIRECTION ( 'NONE',  ( 0.8820010751365664481, 0.000000000000000000, 0.4712473909295847307 ) ) ;
#9258 = FILL_AREA_STYLE ('',( #328 ) ) ;
#9259 = CARTESIAN_POINT ( 'NONE',  ( -2.038881997165930215, -7.478227285005997871, -434.7312091017502667 ) ) ;
#9260 = CARTESIAN_POINT ( 'NONE',  ( 11.54108047910937174, -7.525558156534593479, 314.4999425153565085 ) ) ;
#9261 = CARTESIAN_POINT ( 'NONE',  ( -7.497671121046002973, 10.44264915526000514, 190.0071920248299477 ) ) ;
#9262 = CARTESIAN_POINT ( 'NONE',  ( -26.31853765676889267, -9.000000000000001776, -432.7407288192795249 ) ) ;
#9263 = CARTESIAN_POINT ( 'NONE',  ( 7.083228393897874398, -4.408350100845710884, -525.5349554852709844 ) ) ;
#9264 = CIRCLE ( 'NONE', #187, 10.00000000000000000 ) ;
#9265 = VECTOR ( 'NONE', #10005, 1000.000000000000114 ) ;
#9266 = DIRECTION ( 'NONE',  ( 0.6276613564376926080, 0.000000000000000000, -0.7784864941890744516 ) ) ;
#9267 = DIRECTION ( 'NONE',  ( 0.000000000000000000, -1.000000000000000000, 0.000000000000000000 ) ) ;
#9268 = VERTEX_POINT ( 'NONE', #5579 ) ;
#9269 = CARTESIAN_POINT ( 'NONE',  ( 12.62060098491999938, 8.441142645117002630, 319.9928079742500131 ) ) ;
#9270 = PLANE ( 'NONE',  #4709 ) ;
#9271 = VERTEX_POINT ( 'NONE', #3195 ) ;
#9272 = CARTESIAN_POINT ( 'NONE',  ( -72.90663470102438737, -2.500000000000000000, -371.7168990826883714 ) ) ;
#9273 = VERTEX_POINT ( 'NONE', #9725 ) ;
#9274 = FACE_OUTER_BOUND ( 'NONE', #3546, .T. ) ;
#9275 = AXIS2_PLACEMENT_3D ( 'NONE', #5543, #9049, #8884 ) ;
#9276 = CARTESIAN_POINT ( 'NONE',  ( 14.32792941690000177, -7.389020440446000926, -317.4928077629770087 ) ) ;
#9277 = CARTESIAN_POINT ( 'NONE',  ( -17.12243801299000268, 0.5826713957640000663, -314.8616023057000461 ) ) ;
#9278 = CIRCLE ( 'NONE', #857, 0.5000000000000066613 ) ;
#9279 = LINE ( 'NONE', #508, #6751 ) ;
#9280 = DIRECTION ( 'NONE',  ( 0.000000000000000000, 1.000000000000000000, 0.000000000000000000 ) ) ;
#9281 = ORIENTED_EDGE ( 'NONE', *, *, #2353, .F. ) ;
#9282 = CARTESIAN_POINT ( 'NONE',  ( 1.290325097615000027, -11.49300988401000012, 190.0000000000000000 ) ) ;
#9283 = CARTESIAN_POINT ( 'NONE',  ( -2.000000000000000000, -9.500000000000000000, -409.5000000000000000 ) ) ;
#9284 = EDGE_LOOP ( 'NONE', ( #2576, #10497, #10286, #2512 ) ) ;
#9285 = CARTESIAN_POINT ( 'NONE',  ( -8.833609186824004311, -11.21733050393000575, 191.1197171614399792 ) ) ;
#9286 = DIRECTION ( 'NONE',  ( 0.9942380540931650135, 0.000000000000000000, 0.1071946444232960011 ) ) ;
#9287 = FACE_OUTER_BOUND ( 'NONE', #8347, .T. ) ;
#9288 = CARTESIAN_POINT ( 'NONE',  ( -4.867894159875999271, 12.21747625305000007, 190.4207385301700128 ) ) ;
#9289 = CIRCLE ( 'NONE', #10137, 4.000000000000003553 ) ;
#9290 =( GEOMETRIC_REPRESENTATION_CONTEXT ( 3 ) GLOBAL_UNCERTAINTY_ASSIGNED_CONTEXT ( ( #5601 ) ) GLOBAL_UNIT_ASSIGNED_CONTEXT ( ( #2217, #10483, #6403 ) ) REPRESENTATION_CONTEXT ( 'NONE', 'WORKASPACE' ) );
#9291 = EDGE_CURVE ( 'NONE', #8555, #2824, #3274, .T. ) ;
#9292 = CARTESIAN_POINT ( 'NONE',  ( -0.5403494531946965163, -7.486475365814998284, -434.0354456928992022 ) ) ;
#9293 = SURFACE_STYLE_USAGE ( .BOTH. , #6818 ) ;
#9294 = DIRECTION ( 'NONE',  ( 0.8820010751365675583, 0.000000000000000000, 0.4712473909295827323 ) ) ;
#9295 = CARTESIAN_POINT ( 'NONE',  ( 15.60880606785999980, -7.925821651060998008, 319.5792614743400009 ) ) ;
#9296 = CARTESIAN_POINT ( 'NONE',  ( 14.00000000000000000, -2.500000000000000000, -317.5000000000000000 ) ) ;
#9297 = CARTESIAN_POINT ( 'NONE',  ( 15.10708484062000068, -4.236041382665999500, -315.0848619657999734 ) ) ;
#9298 = CARTESIAN_POINT ( 'NONE',  ( 17.14610219660000112, 0.04370646908745000336, 314.8616023057000461 ) ) ;
#9299 = ORIENTED_EDGE ( 'NONE', *, *, #1577, .T. ) ;
#9300 = CARTESIAN_POINT ( 'NONE',  ( -47.11589368967775471, -7.500000000000000888, -410.8439258096980780 ) ) ;
#9301 = CARTESIAN_POINT ( 'NONE',  ( -19.19790409518002861, 3.716965664678998582, 319.5792614743400009 ) ) ;
#9302 = ADVANCED_FACE ( 'NONE', ( #1662, #8803, #4785 ), #4731, .T. ) ;
#9303 = CARTESIAN_POINT ( 'NONE',  ( -27.98005464532998232, -9.500000000000001776, -417.3300389808354680 ) ) ;
#9304 = CARTESIAN_POINT ( 'NONE',  ( 8.691248314156576171, 8.152891913651146183, 315.0000000000001137 ) ) ;
#9305 = CARTESIAN_POINT ( 'NONE',  ( 7.006889269069000115, -6.844138725329000472, -284.9999999999999432 ) ) ;
#9306 = DIRECTION ( 'NONE',  ( -0.4716280258120416069, 0.000000000000000000, 0.8817975988108813779 ) ) ;
#9307 = DIRECTION ( 'NONE',  ( 0.9942380540931625710, 0.000000000000000000, 0.1071946444233177614 ) ) ;
#9308 = CARTESIAN_POINT ( 'NONE',  ( -18.02719435607597021, -9.500000000000001776, -431.8467903975401896 ) ) ;
#9309 = EDGE_CURVE ( 'NONE', #863, #8555, #6434, .T. ) ;
#9310 = CARTESIAN_POINT ( 'NONE',  ( -27.92645732311634532, -9.000000000000001776, -417.8271580078818488 ) ) ;
#9311 = PRODUCT_DEFINITION_SHAPE ( 'NONE', 'NONE',  #10628 ) ;
#9313 = CARTESIAN_POINT ( 'NONE',  ( 18.87182479219000442, -0.3569112016842001522, 190.0071920248299477 ) ) ;
#9312 = AXIS2_PLACEMENT_3D ( 'NONE', #6071, #10217, #8585 ) ;
#9314 = CARTESIAN_POINT ( 'NONE',  ( -1.624818744522249503, -9.500000000000001776, -412.9798331893018712 ) ) ;
#9315 = CARTESIAN_POINT ( 'NONE',  ( 6.052780067456072999, -5.500000000000000000, -524.2189112390747141 ) ) ;
#9316 = VECTOR ( 'NONE', #1480, 1000.000000000000000 ) ;
#9317 = DIRECTION ( 'NONE',  ( -3.596898300242126276E-07, -0.9999999999999354960, -1.311545752197542526E-22 ) ) ;
#9318 = AXIS2_PLACEMENT_3D ( 'NONE', #5478, #3820, #3012 ) ;
#9319 = ORIENTED_EDGE ( 'NONE', *, *, #1940, .F. ) ;
#9320 = CARTESIAN_POINT ( 'NONE',  ( 15.63927740852997950, 6.344868560643003974, 319.9928079742500131 ) ) ;
#9321 = CARTESIAN_POINT ( 'NONE',  ( -87.43676691142619006, -2.500000000000000000, -348.7659131681800773 ) ) ;
#9322 = LINE ( 'NONE', #393, #5345 ) ;
#9323 = EDGE_LOOP ( 'NONE', ( #8953, #2238, #3904, #6970 ) ) ;
#9324 = FACE_OUTER_BOUND ( 'NONE', #618, .T. ) ;
#9325 = CARTESIAN_POINT ( 'NONE',  ( -6.380917221297004005, -11.42904134337998734, -317.5770954168139610 ) ) ;
#9326 = AXIS2_PLACEMENT_3D ( 'NONE', #51, #5786, #7251 ) ;
#9327 = CARTESIAN_POINT ( 'NONE',  ( -17.35381917807999841, -0.3185724951638000402, -314.6383426456000052 ) ) ;
#9328 = CARTESIAN_POINT ( 'NONE',  ( 9.017403168879978281, 8.607149246413721144, -314.5455549245388056 ) ) ;
#9329 = B_SPLINE_SURFACE_WITH_KNOTS ( 'NONE', 3, 3, ( 
 ( #7038, #1224, #6218, #5256 ),
 ( #8530, #374, #423, #2038 ),
 ( #9402, #3701, #9451, #8907 ),
 ( #797, #5678, #8101, #8000 ),
 ( #5573, #10409, #3217, #7144 ),
 ( #8856, #4881, #4726, #9660 ),
 ( #6493, #3268, #3864, #5515 ),
 ( #5626, #10515, #7141, #7246 ),
 ( #9607, #7354, #6546, #3965 ),
 ( #2248, #7303, #1608, #3050 ),
 ( #6319, #584, #8797, #1438 ),
 ( #4075, #9825, #10463, #639 ),
 ( #1551, #5462, #3915, #7194 ),
 ( #3103, #6379, #2411, #2301 ),
 ( #3160, #1497, #6436, #4777 ),
 ( #9719, #4022, #4830, #8741 ),
 ( #1383, #8045, #8159, #8965 ),
 ( #695, #743, #2359, #10575 ),
 ( #7942, #4667, #9771, #1057 ),
 ( #8366, #8208, #4131, #2465 ),
 ( #9881, #7406, #4342, #5033 ),
 ( #2625, #3540, #8418, #7616 ),
 ( #1871, #2681, #6707, #8260 ),
 ( #897, #846, #263, #6817 ),
 ( #9128, #9931, #5889, #5836 ),
 ( #5732, #5950, #2569, #207 ),
 ( #9239, #9020, #3428, #4291 ),
 ( #3320, #5142, #7564, #9984 ),
 ( #9185, #3485, #6765, #2518 ),
 ( #6601, #1762, #1656, #10039 ),
 ( #4931, #8315, #4184, #1712 ),
 ( #952, #1820, #45, #5086 ),
 ( #5782, #4239, #6654, #1004 ),
 ( #7511, #153, #9073, #7459 ) ),
 .UNSPECIFIED., .F., .F., .F.,
 ( 4, 1, 1, 1, 1, 1, 1, 1, 1, 1, 1, 1, 1, 1, 1, 1, 1, 1, 1, 1, 1, 1, 1, 1, 1, 1, 1, 1, 1, 1, 1, 4 ),
 ( 4, 4 ),
 ( -0.01574130609828000224, 0.000000000000000000, 0.03448275862069000164, 0.06896551724138000328, 0.1034482758621000087, 0.1379310344828000023, 0.1724137931033999926, 0.2068965517240999863, 0.2413793103448000077, 0.2758620689655000291, 0.3103448275861999672, 0.3448275862069000164, 0.3793103448276000100, 0.4137931034483000037, 0.4482758620689999973, 0.4827586206897000465, 0.5172413793103000090, 0.5517241379310000582, 0.5862068965516999963, 0.6206896551723999345, 0.6551724137930999836, 0.6896551724138000328, 0.7241379310344999709, 0.7586206896552000201, 0.7931034482758999582, 0.8275862068966000074, 0.8620689655171999144, 0.8965517241379000746, 0.9310344827586000127, 0.9655172413793000619, 1.000000000000000000, 1.014026462982999810 ),
 ( -0.1697239316932999953, 1.169834029081999960 ),
 .UNSPECIFIED. ) ;
#9330 = EDGE_LOOP ( 'NONE', ( #8323, #8902, #5235, #7713 ) ) ;
#9331 = SURFACE_STYLE_FILL_AREA ( #7661 ) ;
#9332 = CARTESIAN_POINT ( 'NONE',  ( -15.66137281426499861, -7.786477173011506991, 319.0000000000003979 ) ) ;
#9333 = ADVANCED_FACE ( 'NONE', ( #3109 ), #4431, .F. ) ;
#9334 = ORIENTED_EDGE ( 'NONE', *, *, #2723, .T. ) ;
#9335 = FACE_OUTER_BOUND ( 'NONE', #9751, .T. ) ;
#9336 = ORIENTED_EDGE ( 'NONE', *, *, #3614, .F. ) ;
#9337 = CARTESIAN_POINT ( 'NONE',  ( 10.23467949614885164, -10.00000000050611781, -302.4999999999996589 ) ) ;
#9338 = CARTESIAN_POINT ( 'NONE',  ( -18.87259549714001139, 0.3457787829170000937, -302.5071922382879279 ) ) ;
#9339 = CARTESIAN_POINT ( 'NONE',  ( 6.108404012864005139, 11.90988283206001519, 191.1197171614399792 ) ) ;
#9340 = AXIS2_PLACEMENT_3D ( 'NONE', #8254, #893, #259 ) ;
#9341 = CARTESIAN_POINT ( 'NONE',  ( -51.72607275331812104, -12.00000000000000000, -370.6966883942067739 ) ) ;
#9342 =( NAMED_UNIT ( * ) PLANE_ANGLE_UNIT ( ) SI_UNIT ( $, .RADIAN. ) );
#9343 = CARTESIAN_POINT ( 'NONE',  ( -56.92031869107000119, 2.500000000000000000, -403.1217184488000385 ) ) ;
#9344 = CARTESIAN_POINT ( 'NONE',  ( -20.08924610253000509, -0.07535283344304002928, 319.5792614743400009 ) ) ;
#9345 = CARTESIAN_POINT ( 'NONE',  ( 16.55686070535999832, -1.955716293870999767, -315.0848619657999734 ) ) ;
#9346 = CARTESIAN_POINT ( 'NONE',  ( -8.551447359560999217, 8.144527334518999240, 315.0848619657999734 ) ) ;
#9347 = EDGE_LOOP ( 'NONE', ( #5330, #3623, #2814, #2977 ) ) ;
#9348 = AXIS2_PLACEMENT_3D ( 'NONE', #7963, #1465, #7007 ) ;
#9349 = CARTESIAN_POINT ( 'NONE',  ( -72.90663470102438737, -2.599999999999984102, -368.2168990826883146 ) ) ;
#9350 = ORIENTED_EDGE ( 'NONE', *, *, #5835, .T. ) ;
#9351 = CARTESIAN_POINT ( 'NONE',  ( -19.49027688392999735, 2.831154404542999714, 318.8802828394900644 ) ) ;
#9352 = AXIS2_PLACEMENT_3D ( 'NONE', #8333, #4204, #7579 ) ;
#9353 = VECTOR ( 'NONE', #6834, 1000.000000000000000 ) ;
#9354 = CARTESIAN_POINT ( 'NONE',  ( -5.563766465756743607, -8.000000000000000000, -337.3048648817380126 ) ) ;
#9355 = LINE ( 'NONE', #1990, #5701 ) ;
#9356 = CARTESIAN_POINT ( 'NONE',  ( -15.00000000000071587, -0.4945770392355663403, 315.0000000000001705 ) ) ;
#9357 = AXIS2_PLACEMENT_3D ( 'NONE', #2174, #723, #8718 ) ;
#9358 = VECTOR ( 'NONE', #4008, 1000.000000000000114 ) ;
#9359 = FACE_OUTER_BOUND ( 'NONE', #8663, .T. ) ;
#9360 = CIRCLE ( 'NONE', #6091, 12.49999999999998046 ) ;
#9361 = FILL_AREA_STYLE_COLOUR ( '', #6599 ) ;
#9362 = DIRECTION ( 'NONE',  ( 0.000000000000000000, -1.000000000000000000, 0.000000000000000000 ) ) ;
#9363 = CARTESIAN_POINT ( 'NONE',  ( -16.53772850381891857, 2.187491735906824442, -315.0000000000001137 ) ) ;
#9364 = CARTESIAN_POINT ( 'NONE',  ( 5.890130794754004029, 10.81842929378999330, 190.0071920248299477 ) ) ;
#9365 = FACE_BOUND ( 'NONE', #8612, .T. ) ;
#9366 = CARTESIAN_POINT ( 'NONE',  ( 10.21957842388999893, -9.686567771335999666, -317.5000000000000000 ) ) ;
#9367 =( GEOMETRIC_REPRESENTATION_CONTEXT ( 3 ) GLOBAL_UNCERTAINTY_ASSIGNED_CONTEXT ( ( #17 ) ) GLOBAL_UNIT_ASSIGNED_CONTEXT ( ( #9490, #5398, #10448 ) ) REPRESENTATION_CONTEXT ( 'NONE', 'WORKASPACE' ) );
#9368 = EDGE_CURVE ( 'NONE', #1376, #9105, #7610, .T. ) ;
#9369 = CARTESIAN_POINT ( 'NONE',  ( 8.355542331113237964, -5.750853016826391162, -525.7099095707894776 ) ) ;
#9370 = CARTESIAN_POINT ( 'NONE',  ( 12.75139817577315604, -6.274227700150676768, 315.0000000000000568 ) ) ;
#9371 = CARTESIAN_POINT ( 'NONE',  ( 3.903842856253999738, 9.647088721075000706, -314.6383426456000052 ) ) ;
#9372 = EDGE_LOOP ( 'NONE', ( #10555, #9064, #1703, #9890, #3299 ) ) ;
#9373 = CARTESIAN_POINT ( 'NONE',  ( 14.24138406224000342, 7.443131114976996976, 319.9928079742500131 ) ) ;
#9374 = CARTESIAN_POINT ( 'NONE',  ( -38.85901494634669007, -8.000000000000000000, -386.6556615250812570 ) ) ;
#9375 = CARTESIAN_POINT ( 'NONE',  ( -56.92031869107000119, -2.500000000000000000, -403.1217184488000385 ) ) ;
#9376 = VERTEX_POINT ( 'NONE', #3154 ) ;
#9377 = CARTESIAN_POINT ( 'NONE',  ( -16.09890757810000750, 5.925814185855000638, -317.4928077629770087 ) ) ;
#9378 = CARTESIAN_POINT ( 'NONE',  ( 6.769722431736004076, -11.85293133419998846, -317.0792622552969533 ) ) ;
#9379 = ADVANCED_FACE ( 'NONE', ( #1492 ), #6539, .F. ) ;
#9380 = CARTESIAN_POINT ( 'NONE',  ( -17.14577796628000073, 0.02050488658304000164, -314.8616023057000461 ) ) ;
#9381 = EDGE_CURVE ( 'NONE', #9889, #8268, #7802, .T. ) ;
#9382 = DIRECTION ( 'NONE',  ( -0.1124491875265152124, 0.000000000000000000, 0.9936574763089273121 ) ) ;
#9383 = VERTEX_POINT ( 'NONE', #5564 ) ;
#9384 = DIRECTION ( 'NONE',  ( 1.000000000000000000, 0.000000000000000000, 0.000000000000000000 ) ) ;
#9385 = ORIENTED_EDGE ( 'NONE', *, *, #172, .F. ) ;
#9386 = CARTESIAN_POINT ( 'NONE',  ( 6.403271823880001712, -11.84773780780999530, 191.1197171614399792 ) ) ;
#9387 = VERTEX_POINT ( 'NONE', #5620 ) ;
#9388 = CARTESIAN_POINT ( 'NONE',  ( -43.46674421124934184, -7.500000000000000888, -402.7790142173016648 ) ) ;
#9389 = CARTESIAN_POINT ( 'NONE',  ( -11.24500836742999610, -9.126642939585995151, -302.5071922382879279 ) ) ;
#9390 = CYLINDRICAL_SURFACE ( 'NONE', #2664, 0.5000000000000079936 ) ;
#9391 = EDGE_CURVE ( 'NONE', #5334, #5915, #435, .T. ) ;
#9392 = CARTESIAN_POINT ( 'NONE',  ( -1.554031834198139839, -7.468176060817003581, -434.5954497281065301 ) ) ;
#9393 = CARTESIAN_POINT ( 'NONE',  ( 8.965618380443995505, 10.00899073891999436, -302.5071922382879279 ) ) ;
#9394 = CARTESIAN_POINT ( 'NONE',  ( -19.78455541125000750, -1.880268586931002073, 318.8802828394900644 ) ) ;
#9395 = CARTESIAN_POINT ( 'NONE',  ( 17.43193685618000188, -1.405086463480999859, -314.4150829855000211 ) ) ;
#9396 = CARTESIAN_POINT ( 'NONE',  ( -17.43193685618000188, 1.405086463480999859, 314.4150829855000211 ) ) ;
#9397 = EDGE_LOOP ( 'NONE', ( #4058, #403, #7279, #10067, #4642, #6353, #4523, #8868, #9118, #7467, #5076, #5776, #7665, #9994, #2984, #3785, #5521 ) ) ;
#9398 = CARTESIAN_POINT ( 'NONE',  ( 1.205561540619000116, -11.37600766585000933, 190.0071920248299477 ) ) ;
#9399 = ORIENTED_EDGE ( 'NONE', *, *, #543, .T. ) ;
#9400 = CARTESIAN_POINT ( 'NONE',  ( -14.74960734804001916, 8.445183187697006488, 318.8802828394900644 ) ) ;
#9401 = DIRECTION ( 'NONE',  ( 1.000000000000000000, 0.000000000000000000, 0.000000000000000000 ) ) ;
#9402 = CARTESIAN_POINT ( 'NONE',  ( -16.92248268936999978, -0.04189409840125999512, 315.0848619657999734 ) ) ;
#9403 = CIRCLE ( 'NONE', #140, 0.7500000000000247580 ) ;
#9404 = DIRECTION ( 'NONE',  ( -0.2381566825879641303, -3.988721798185001137E-09, 0.9712267472319199291 ) ) ;
#9405 = CARTESIAN_POINT ( 'NONE',  ( -20.00000000032979131, -7.322330470066152230, 319.0000000000000568 ) ) ;
#9406 = CARTESIAN_POINT ( 'NONE',  ( -15.35654050466420983, -4.050078947852131073, -315.0000000000000568 ) ) ;
#9407 = CARTESIAN_POINT ( 'NONE',  ( -8.155631454398118763, -3.591146263826743290, -437.6540831751978544 ) ) ;
#9408 = DIRECTION ( 'NONE',  ( 1.000000000000000000, 0.000000000000000000, 0.000000000000000000 ) ) ;
#9409 = CARTESIAN_POINT ( 'NONE',  ( -17.49999999999999289, 5.867334123212277319, -302.5000000000003411 ) ) ;
#9410 = CARTESIAN_POINT ( 'NONE',  ( -13.97602275805729199, 5.383336353019481102, -315.0000000000000568 ) ) ;
#9411 = CARTESIAN_POINT ( 'NONE',  ( 11.56561186376999295, 8.976555918559004255, 190.0071920248299477 ) ) ;
#9412 = DIRECTION ( 'NONE',  ( 0.1247904863035890072, 0.000000000000000000, -0.9921831154218024862 ) ) ;
#9413 = CARTESIAN_POINT ( 'NONE',  ( 2.034678270035999770, -11.44985799554000039, -317.5000000000000000 ) ) ;
#9414 = EDGE_CURVE ( 'NONE', #10567, #9606, #5227, .T. ) ;
#9415 = DIRECTION ( 'NONE',  ( 1.000000000000000000, 0.000000000000000000, 0.000000000000000000 ) ) ;
#9416 = DIRECTION ( 'NONE',  ( 0.000000000000000000, 0.000000000000000000, 1.000000000000000000 ) ) ;
#9417 = CARTESIAN_POINT ( 'NONE',  ( 13.82226565756009684, -5.505830577453552088, 315.0000000000000568 ) ) ;
#9418 = CARTESIAN_POINT ( 'NONE',  ( 10.58801790939999954, 8.088125079530000150, -314.4150829855000211 ) ) ;
#9419 = ORIENTED_EDGE ( 'NONE', *, *, #1759, .T. ) ;
#9420 = DIRECTION ( 'NONE',  ( 0.000000000000000000, 1.000000000000000000, -0.000000000000000000 ) ) ;
#9421 = CARTESIAN_POINT ( 'NONE',  ( -0.5535498271043974849, -7.499999952522999891, -434.2938920418101816 ) ) ;
#9422 = CARTESIAN_POINT ( 'NONE',  ( -77.77979771402830522, -7.500000000000000000, -385.9384419754180158 ) ) ;
#9423 = VERTEX_POINT ( 'NONE', #8850 ) ;
#9424 = CARTESIAN_POINT ( 'NONE',  ( -18.99999673287999968, 1.191366929371999993E-07, 191.0000000000000000 ) ) ;
#9425 = EDGE_CURVE ( 'NONE', #10392, #563, #8039, .T. ) ;
#9426 = CARTESIAN_POINT ( 'NONE',  ( -7.757100520214003758, -11.09835178152000168, -317.5770954168139610 ) ) ;
#9427 = EDGE_CURVE ( 'NONE', #6833, #7332, #7134, .T. ) ;
#9428 = LINE ( 'NONE', #10438, #3112 ) ;
#9429 = CARTESIAN_POINT ( 'NONE',  ( 15.54698342962804958, 4.499693933759708386, -314.5711572504541778 ) ) ;
#9430 = VERTEX_POINT ( 'NONE', #3042 ) ;
#9431 = AXIS2_PLACEMENT_3D ( 'NONE', #2495, #9154, #9907 ) ;
#9432 = CARTESIAN_POINT ( 'NONE',  ( -17.50000000088854435, -5.867334121986939266, 189.9999999999997442 ) ) ;
#9433 = ORIENTED_EDGE ( 'NONE', *, *, #1252, .F. ) ;
#9434 = CARTESIAN_POINT ( 'NONE',  ( -4.466162596268001828, -12.19410025049000446, 191.1197171614399792 ) ) ;
#9435 = ORIENTED_EDGE ( 'NONE', *, *, #5848, .F. ) ;
#9436 = CARTESIAN_POINT ( 'NONE',  ( -18.02719435607597021, -9.633703999999999823, -431.8467903975401896 ) ) ;
#9437 = CARTESIAN_POINT ( 'NONE',  ( -14.00000000000000000, -2.500000000000000000, -317.5000000000000000 ) ) ;
#9438 = EDGE_CURVE ( 'NONE', #2509, #1953, #576, .T. ) ;
#9439 = FACE_OUTER_BOUND ( 'NONE', #7009, .T. ) ;
#9440 = AXIS2_PLACEMENT_3D ( 'NONE', #7961, #8705, #4631 ) ;
#9441 = CARTESIAN_POINT ( 'NONE',  ( -0.7362249915901031283, -7.501925031340999084, -434.1840766770703226 ) ) ;
#9442 = CARTESIAN_POINT ( 'NONE',  ( 10.13603924037000326, 9.590552501249007378, -302.5071922382879279 ) ) ;
#9443 = CARTESIAN_POINT ( 'NONE',  ( -19.86662547467000550, -1.900306748470001139, 319.5792614743400009 ) ) ;
#9444 = CARTESIAN_POINT ( 'NONE',  ( 17.35381917807999841, 0.3185724951638000402, -314.6383426456000052 ) ) ;
#9445 = CARTESIAN_POINT ( 'NONE',  ( -10.40890489166000066, 7.434429060800999522, 315.0848619657999734 ) ) ;
#9446 = ORIENTED_EDGE ( 'NONE', *, *, #9035, .F. ) ;
#9447 = CARTESIAN_POINT ( 'NONE',  ( -4.308829118669001979, -11.09213725138999962, 190.0071920248299477 ) ) ;
#9448 = ORIENTED_EDGE ( 'NONE', *, *, #8843, .T. ) ;
#9449 = CARTESIAN_POINT ( 'NONE',  ( 1.327417525529001496, 12.48520226272998990, 318.8802828394900644 ) ) ;
#9450 = FACE_OUTER_BOUND ( 'NONE', #5021, .T. ) ;
#9451 = CARTESIAN_POINT ( 'NONE',  ( -17.36972170382999892, -0.04551883977363000572, 314.6383426456000052 ) ) ;
#9452 = DIRECTION ( 'NONE',  ( 0.9902680687415800209, 0.000000000000000000, 0.1391731009599966873 ) ) ;
#9453 = CARTESIAN_POINT ( 'NONE',  ( -86.86306229143158930, -2.500000000000000000, -370.6132103076870976 ) ) ;
#9454 = CARTESIAN_POINT ( 'NONE',  ( -11.65180110541762382, -6.897852064324583310, -314.9999999999999432 ) ) ;
#9455 = CARTESIAN_POINT ( 'NONE',  ( 20.00000000000000355, 25.00000000015544543, 319.0000000000000000 ) ) ;
#9456 = DIRECTION ( 'NONE',  ( 0.8820010751365653379, 0.000000000000000000, 0.4712473909295871732 ) ) ;
#9457 = CARTESIAN_POINT ( 'NONE',  ( 17.50000000000000711, -8.653813013134384923E-10, -302.5000000000000568 ) ) ;
#9458 = CARTESIAN_POINT ( 'NONE',  ( -4.252979419060009647, 9.197563690522738256, -315.0000000000001137 ) ) ;
#9459 = CARTESIAN_POINT ( 'NONE',  ( -18.89081873304001036, 0.08752760549136004431, 190.0071920248299477 ) ) ;
#9460 = CARTESIAN_POINT ( 'NONE',  ( 17.44863594430761111, 0.8973220660537315485, 314.4999502393481521 ) ) ;
#9461 = VERTEX_POINT ( 'NONE', #9765 ) ;
#9462 = CARTESIAN_POINT ( 'NONE',  ( -10.11497662670000075, -9.727801543432001097, -317.5000000000000000 ) ) ;
#9463 = DIRECTION ( 'NONE',  ( 0.000000000000000000, -1.000000000000000000, 0.000000000000000000 ) ) ;
#9464 = CARTESIAN_POINT ( 'NONE',  ( 15.26162423979700300, -4.160529437000930031, 314.9999999999999432 ) ) ;
#9465 = CARTESIAN_POINT ( 'NONE',  ( 8.519003879469000395, 8.390442916014999142, -314.8616023057000461 ) ) ;
#9466 = FACE_BOUND ( 'NONE', #356, .T. ) ;
#9467 = AXIS2_PLACEMENT_3D ( 'NONE', #853, #2472, #9028 ) ;
#9468 = FACE_OUTER_BOUND ( 'NONE', #7021, .T. ) ;
#9469 = CARTESIAN_POINT ( 'NONE',  ( 4.000000000000000000, 2.500000000000000000, -410.4979246179000256 ) ) ;
#9470 = CARTESIAN_POINT ( 'NONE',  ( -72.90663470102438737, -12.50000000000000000, -371.7168990826883714 ) ) ;
#9471 = ORIENTED_EDGE ( 'NONE', *, *, #5504, .T. ) ;
#9472 = CARTESIAN_POINT ( 'NONE',  ( 19.46050885281001896, 1.651188223417001444, -317.5770954168139610 ) ) ;
#9473 = CARTESIAN_POINT ( 'NONE',  ( -1.606003227921999343, -12.55439432250999587, -317.0792622552969533 ) ) ;
#9474 = PRODUCT_DEFINITION_SHAPE ( 'NONE', 'NONE',  #8885 ) ;
#9475 = CIRCLE ( 'NONE', #3302, 3.400000000000014122 ) ;
#9476 = CARTESIAN_POINT ( 'NONE',  ( 14.00000000000000000, 2.500000000000000000, -272.5000000000000000 ) ) ;
#9477 = CIRCLE ( 'NONE', #2449, 0.5000000000000128786 ) ;
#9478 = LINE ( 'NONE', #6094, #4687 ) ;
#9479 = VERTEX_POINT ( 'NONE', #687 ) ;
#9480 = CARTESIAN_POINT ( 'NONE',  ( -9.616122863433998802, -9.909251266138999981, 190.0000000000000000 ) ) ;
#9481 = CARTESIAN_POINT ( 'NONE',  ( -12.21612826667444374, -9.907025583609534891, 319.0000000000003979 ) ) ;
#9482 = ORIENTED_EDGE ( 'NONE', *, *, #1305, .T. ) ;
#9483 = LINE ( 'NONE', #4481, #5339 ) ;
#9484 = ORIENTED_EDGE ( 'NONE', *, *, #8809, .T. ) ;
#9485 = DIRECTION ( 'NONE',  ( 0.000000000000000000, 1.000000000000000000, 0.000000000000000000 ) ) ;
#9486 = DIRECTION ( 'NONE',  ( -0.1071946444232964035, 0.000000000000000000, 0.9942380540931649024 ) ) ;
#9487 = CARTESIAN_POINT ( 'NONE',  ( 20.00478054794001537, 0.07382975964161003768, 191.1197171614399792 ) ) ;
#9488 = AXIS2_PLACEMENT_3D ( 'NONE', #2973, #9638, #10552 ) ;
#9489 = CARTESIAN_POINT ( 'NONE',  ( -0.7659865709275307522, -7.501556614171002835, -434.2093659254040858 ) ) ;
#9490 =( LENGTH_UNIT ( ) NAMED_UNIT ( * ) SI_UNIT ( .MILLI., .METRE. ) );
#9491 = EDGE_CURVE ( 'NONE', #3077, #5506, #2489, .T. ) ;
#9492 = CARTESIAN_POINT ( 'NONE',  ( 19.60176101890002442, 0.3495461351719001408, -302.4229045757450081 ) ) ;
#9493 = CARTESIAN_POINT ( 'NONE',  ( -6.490016473005998598, -11.91548699335000272, 319.5792614743400009 ) ) ;
#9494 = CARTESIAN_POINT ( 'NONE',  ( 13.24479143485999977, -5.858166912337999577, -315.0848619657999734 ) ) ;
#9495 = CARTESIAN_POINT ( 'NONE',  ( -8.620760283086999820, 8.357092890497000326, 314.8616023057000461 ) ) ;
#9496 = EDGE_CURVE ( 'NONE', #4386, #8331, #1981, .T. ) ;
#9497 = ORIENTED_EDGE ( 'NONE', *, *, #9823, .F. ) ;
#9498 = CARTESIAN_POINT ( 'NONE',  ( -19.51240441859933838, -2.792009854621256171, 190.9999999999995737 ) ) ;
#9499 = CARTESIAN_POINT ( 'NONE',  ( 10.18759338605000409, 10.75836373329000217, 318.8802828394900644 ) ) ;
#9500 = DIRECTION ( 'NONE',  ( 0.000000000000000000, 1.000000000000000000, -0.000000000000000000 ) ) ;
#9501 = VECTOR ( 'NONE', #9234, 1000.000000000000000 ) ;
#9502 = ADVANCED_FACE ( 'NONE', ( #6647 ), #9120, .F. ) ;
#9503 = DIRECTION ( 'NONE',  ( 0.000000000000000000, -1.000000000000000000, 0.000000000000000000 ) ) ;
#9504 = DIRECTION ( 'NONE',  ( -0.9612616959383299964, 0.000000000000000000, -0.2756373558169601945 ) ) ;
#9505 = DIRECTION ( 'NONE',  ( 0.000000000000000000, -1.000000000000000000, 0.000000000000000000 ) ) ;
#9506 = CARTESIAN_POINT ( 'NONE',  ( 19.99999999999999289, -7.322330470418032533, 319.0000000000000568 ) ) ;
#9507 = CARTESIAN_POINT ( 'NONE',  ( -16.25556775813545585, -2.760696635281385092, -315.0000000000000000 ) ) ;
#9508 = DIRECTION ( 'NONE',  ( 0.3420201433256988555, 0.000000000000000000, -0.9396926207858975477 ) ) ;
#9509 = CARTESIAN_POINT ( 'NONE',  ( -81.20226567874760804, -7.500000000000000000, -347.7024309728756748 ) ) ;
#9510 = AXIS2_PLACEMENT_3D ( 'NONE', #1624, #809, #4092 ) ;
#9511 = CLOSED_SHELL ( 'NONE', ( #9113, #3719, #1617, #4153, #7722, #10524, #2778, #888, #7653, #7140 ) ) ;
#9512 = CARTESIAN_POINT ( 'NONE',  ( 0.3940538687071376001, 9.499927474253876625, -315.0000000000000568 ) ) ;
#9513 = CARTESIAN_POINT ( 'NONE',  ( 7.457264729102998757, 11.17642278912000720, 189.9229057364800042 ) ) ;
#9514 = CARTESIAN_POINT ( 'NONE',  ( 13.64771696944629475, 6.290639922060250910, 314.4999474536516004 ) ) ;
#9515 = ORIENTED_EDGE ( 'NONE', *, *, #3125, .F. ) ;
#9516 = CARTESIAN_POINT ( 'NONE',  ( -3.336936413097000287, -11.33398029193999967, -317.5000000000000000 ) ) ;
#9517 = AXIS2_PLACEMENT_3D ( 'NONE', #5925, #132, #9052 ) ;
#9518 = VECTOR ( 'NONE', #327, 1000.000000000000000 ) ;
#9519 = LINE ( 'NONE', #2209, #1593 ) ;
#9520 = EDGE_CURVE ( 'NONE', #2925, #78, #3348, .T. ) ;
#9521 = CARTESIAN_POINT ( 'NONE',  ( 15.40286302630929427, -3.995001727760178145, 315.0000000000000568 ) ) ;
#9522 = CARTESIAN_POINT ( 'NONE',  ( 8.655660348039997842, 8.816209662726999241, -314.4150829855000211 ) ) ;
#9523 = CARTESIAN_POINT ( 'NONE',  ( 2.881524480432390771E-09, -9.999999999999998224, 314.4999507458384755 ) ) ;
#9524 = CARTESIAN_POINT ( 'NONE',  ( -12.76583521038999613, 9.157751700393998107, 320.0770942683900557 ) ) ;
#9525 = CARTESIAN_POINT ( 'NONE',  ( -0.8363673731450661508, -2.571798426227997592, -434.7280016174766502 ) ) ;
#9526 = ORIENTED_EDGE ( 'NONE', *, *, #3251, .T. ) ;
#9527 = CARTESIAN_POINT ( 'NONE',  ( 11.49606901914998858, 9.781307837508002478, -317.5770954168139610 ) ) ;
#9528 = CARTESIAN_POINT ( 'NONE',  ( -11.49606901914998858, -9.781307837508002478, -317.5770954168139610 ) ) ;
#9529 = CARTESIAN_POINT ( 'NONE',  ( -17.50000000000000000, -0.7437989020623000380, -315.0000000000000000 ) ) ;
#9530 = CARTESIAN_POINT ( 'NONE',  ( -15.54345086749721716, 4.503564883714276768, -314.5712070352258820 ) ) ;
#9531 = VERTEX_POINT ( 'NONE', #10030 ) ;
#9532 = CARTESIAN_POINT ( 'NONE',  ( -9.801682940292002044, 9.841837802148999614, 190.0000000000000000 ) ) ;
#9533 = MECHANICAL_DESIGN_GEOMETRIC_PRESENTATION_REPRESENTATION (  '', ( #784 ), #5931 ) ;
#9534 = CARTESIAN_POINT ( 'NONE',  ( -6.473926368715491542, -11.84005611832666283, 319.0000000000003979 ) ) ;
#9535 = VERTEX_POINT ( 'NONE', #7399 ) ;
#9536 = CARTESIAN_POINT ( 'NONE',  ( 6.468659092862918847, 11.84071280232868695, -316.5000000000004547 ) ) ;
#9537 = ORIENTED_EDGE ( 'NONE', *, *, #9204, .F. ) ;
#9538 = DIRECTION ( 'NONE',  ( -0.8820010751365675583, 0.000000000000000000, -0.4712473909295827323 ) ) ;
#9539 = CARTESIAN_POINT ( 'NONE',  ( 9.124390749379998056, -10.69353917616999539, -302.4229045757450081 ) ) ;
#9540 = CARTESIAN_POINT ( 'NONE',  ( 13.01115177740000384, 9.495820311550003723, 191.1197171614399792 ) ) ;
#9541 = CARTESIAN_POINT ( 'NONE',  ( -0.3010101818115299976, -7.537189068435002248, -434.2310189891967411 ) ) ;
#9542 = EDGE_CURVE ( 'NONE', #8191, #8559, #5078, .T. ) ;
#9543 = CARTESIAN_POINT ( 'NONE',  ( 3.563286991701002382, 11.18699815210999660, -302.5071922382879279 ) ) ;
#9544 = LINE ( 'NONE', #7084, #7719 ) ;
#9545 = CARTESIAN_POINT ( 'NONE',  ( 6.537559671572000575, -9.400791339334000796, -314.4150829855000211 ) ) ;
#9546 = CARTESIAN_POINT ( 'NONE',  ( -16.99702983282000091, 1.298346578676000007, 314.8616023057000461 ) ) ;
#9547 = VERTEX_POINT ( 'NONE', #5132 ) ;
#9548 = FACE_OUTER_BOUND ( 'NONE', #5123, .T. ) ;
#9549 = CARTESIAN_POINT ( 'NONE',  ( -1.034036475800059751, -7.475296907637412502, -434.4283210023707511 ) ) ;
#9550 = FACE_OUTER_BOUND ( 'NONE', #9215, .T. ) ;
#9551 = APPLICATION_CONTEXT ( 'automotive_design' ) ;
#9552 = EDGE_CURVE ( 'NONE', #3871, #7563, #4975, .T. ) ;
#9553 = ADVANCED_FACE ( 'NONE', ( #1753 ), #4925, .F. ) ;
#9554 = ORIENTED_EDGE ( 'NONE', *, *, #810, .T. ) ;
#9555 = LINE ( 'NONE', #7732, #8531 ) ;
#9556 = CARTESIAN_POINT ( 'NONE',  ( -15.44313366109816599, 3.946504251847836819, 315.0000000000000568 ) ) ;
#9557 = FACE_OUTER_BOUND ( 'NONE', #8775, .T. ) ;
#9558 = CARTESIAN_POINT ( 'NONE',  ( -4.532042191365901473, -9.152867265080528725, -315.0000000000000568 ) ) ;
#9559 = CARTESIAN_POINT ( 'NONE',  ( -38.59226537204000351, 2.500000000000000000, -500.7880554352000217 ) ) ;
#9560 = CARTESIAN_POINT ( 'NONE',  ( -56.92031869107000119, -2.500000000000000000, -403.1217184488000385 ) ) ;
#9561 = DIRECTION ( 'NONE',  ( 0.9942380540931649024, 0.000000000000000000, 0.1071946444232959872 ) ) ;
#9562 = CARTESIAN_POINT ( 'NONE',  ( 1.669371716897545488, 9.454742746653563401, -315.0000000000000000 ) ) ;
#9563 = PRODUCT_DEFINITION_SHAPE ( 'NONE', 'NONE',  #10634 ) ;
#9564 = CARTESIAN_POINT ( 'NONE',  ( 14.56080423438999993, 8.072998568875000558, 189.9229057364800042 ) ) ;
#9565 = DIRECTION ( 'NONE',  ( 0.8126105599114364919, 0.000000000000000000, -0.5828070674935419415 ) ) ;
#9566 = EDGE_CURVE ( 'NONE', #4172, #6718, #1110, .T. ) ;
#9567 = AXIS2_PLACEMENT_3D ( 'NONE', #324, #3648, #2089 ) ;
#9568 = CARTESIAN_POINT ( 'NONE',  ( 18.99984327789000105, -0.5550485914519999175, -317.4999999998989892 ) ) ;
#9569 = CARTESIAN_POINT ( 'NONE',  ( 1.525345003100600394, -7.500000000000000000, -348.4143162901089568 ) ) ;
#9570 = CARTESIAN_POINT ( 'NONE',  ( -239.2452716288999568, -4.999999999999999112, -54.02631980576001069 ) ) ;
#9571 = CARTESIAN_POINT ( 'NONE',  ( 8.636532331090950976, -8.171139803988637595, 315.0000000000000568 ) ) ;
#9572 = ORIENTED_EDGE ( 'NONE', *, *, #1807, .F. ) ;
#9573 =( BOUNDED_CURVE ( )  B_SPLINE_CURVE ( 3, ( #9813, #9117, #4226, #8149 ),
 .UNSPECIFIED., .F., .F. ) 
 B_SPLINE_CURVE_WITH_KNOTS ( ( 4, 4 ),
 ( 0.000000000000000000, 1.000000000000000000 ),
 .UNSPECIFIED. ) 
 CURVE ( )  GEOMETRIC_REPRESENTATION_ITEM ( )  RATIONAL_B_SPLINE_CURVE ( ( 1.171566417337515764, 0.9428088753385223120, 0.9428111942444009630, 1.171573374055151495 ) ) 
 REPRESENTATION_ITEM ( '' )  );
#9574 = CARTESIAN_POINT ( 'NONE',  ( 14.23799507159000122, 5.083276007328000112, -315.0848619657999734 ) ) ;
#9575 = CARTESIAN_POINT ( 'NONE',  ( 17.59656075795390606, 5.807225057570236437, 314.4999507458385324 ) ) ;
#9576 = VECTOR ( 'NONE', #3380, 1000.000000000000227 ) ;
#9577 = CARTESIAN_POINT ( 'NONE',  ( -19.57081977481000834, -0.3814303831828999014, 320.0770942683900557 ) ) ;
#9578 = CARTESIAN_POINT ( 'NONE',  ( -0.9958895184599025896, -7.426437712707262051, -434.8066008177434583 ) ) ;
#9579 = CARTESIAN_POINT ( 'NONE',  ( -0.3079143655542058711, -2.454520757324000435, -434.0165891553489814 ) ) ;
#9580 = EDGE_LOOP ( 'NONE', ( #5845, #3083, #7034, #10440 ) ) ;
#9581 = CARTESIAN_POINT ( 'NONE',  ( 18.28030995243001655, 2.924502517761999876, -317.4928077629770087 ) ) ;
#9582 = CARTESIAN_POINT ( 'NONE',  ( -14.92964316144998627, -8.327009966606000901, -316.3802825947000201 ) ) ;
#9583 = DIRECTION ( 'NONE',  ( 0.8820010751365675583, 0.000000000000000000, 0.4712473909295827323 ) ) ;
#9584 = DIRECTION ( 'NONE',  ( -0.3420201433256991330, 0.000000000000000000, 0.9396926207858973257 ) ) ;
#9585 = ORIENTED_EDGE ( 'NONE', *, *, #2992, .T. ) ;
#9586 = CARTESIAN_POINT ( 'NONE',  ( -17.03769437857130598, -2.221013643562866680, -314.5274634404338485 ) ) ;
#9587 = EDGE_LOOP ( 'NONE', ( #7918, #8646, #803, #8975 ) ) ;
#9588 = CARTESIAN_POINT ( 'NONE',  ( -9.374494192145073512, 11.05367988180384842, -316.5000000000004547 ) ) ;
#9589 = ORIENTED_EDGE ( 'NONE', *, *, #2683, .T. ) ;
#9590 = CARTESIAN_POINT ( 'NONE',  ( -15.46063250253144972, -3.925225575964395919, 315.0000000000000568 ) ) ;
#9591 = CARTESIAN_POINT ( 'NONE',  ( -18.91993355959997558, -3.215835268190998075, -302.4229045757450081 ) ) ;
#9592 = LINE ( 'NONE', #3953, #7617 ) ;
#9593 =( NAMED_UNIT ( * ) PLANE_ANGLE_UNIT ( ) SI_UNIT ( $, .RADIAN. ) );
#9594 = CIRCLE ( 'NONE', #7369, 3.400000000000014122 ) ;
#9595 = CARTESIAN_POINT ( 'NONE',  ( 3.702588368219998927, 12.37624192652999966, -302.9207377450070453 ) ) ;
#9596 = DIRECTION ( 'NONE',  ( 0.1247904863035921574, 0.000000000000000000, -0.9921831154218020421 ) ) ;
#9597 = ORIENTED_EDGE ( 'NONE', *, *, #1084, .F. ) ;
#9598 = CARTESIAN_POINT ( 'NONE',  ( -1.257430124576000008, -9.427442400486999219, -315.0848619657999734 ) ) ;
#9599 = CARTESIAN_POINT ( 'NONE',  ( -2.000000000003786749, -9.000000000000001776, -409.4999999999758415 ) ) ;
#9600 = VERTEX_POINT ( 'NONE', #5024 ) ;
#9601 = CARTESIAN_POINT ( 'NONE',  ( -18.89053622393001675, -0.06335528492986002014, 190.0071920248299477 ) ) ;
#9602 = CARTESIAN_POINT ( 'NONE',  ( 16.34828874915077535, 7.214440038016817880, 190.9999999999996589 ) ) ;
#9603 = DIRECTION ( 'NONE',  ( 0.000000000000000000, -1.000000000000000000, 0.000000000000000000 ) ) ;
#9604 = AXIS2_PLACEMENT_3D ( 'NONE', #8457, #2965, #1297 ) ;
#9605 = EDGE_CURVE ( 'NONE', #3194, #1259, #10553, .T. ) ;
#9606 = VERTEX_POINT ( 'NONE', #1702 ) ;
#9607 = CARTESIAN_POINT ( 'NONE',  ( -15.07109120124999890, -4.275483045295999318, 315.0848619657999734 ) ) ;
#9608 =( NAMED_UNIT ( * ) SI_UNIT ( $, .STERADIAN. ) SOLID_ANGLE_UNIT ( ) );
#9609 = CARTESIAN_POINT ( 'NONE',  ( -15.63367387165999922, 6.510275065263000371, 320.0000000000000000 ) ) ;
#9610 = CARTESIAN_POINT ( 'NONE',  ( -9.801936311039993299, -9.714404437230999889, 319.9928079742500131 ) ) ;
#9611 = AXIS2_PLACEMENT_3D ( 'NONE', #3444, #3552, #6780 ) ;
#9612 = CARTESIAN_POINT ( 'NONE',  ( -15.44329739658678058, -3.946306641738667409, -314.9999999999999432 ) ) ;
#9613 = CARTESIAN_POINT ( 'NONE',  ( -10.00000000000000000, -2.500000000000000000, -315.0000000000000000 ) ) ;
#9614 = ORIENTED_EDGE ( 'NONE', *, *, #7911, .T. ) ;
#9615 = LINE ( 'NONE', #3111, #7079 ) ;
#9616 = EDGE_CURVE ( 'NONE', #1218, #8561, #8304, .T. ) ;
#9617 = CARTESIAN_POINT ( 'NONE',  ( -16.39637408479998726, 7.274214857915000998, 190.4207385301700128 ) ) ;
#9618 = CARTESIAN_POINT ( 'NONE',  ( 1.514429654104534930E-09, 10.00000000000000000, 189.9999999999998863 ) ) ;
#9619 = AXIS2_PLACEMENT_3D ( 'NONE', #10459, #9603, #3047 ) ;
#9620 = DIRECTION ( 'NONE',  ( 0.000000000000000000, 0.000000000000000000, -1.000000000000000000 ) ) ;
#9621 = CARTESIAN_POINT ( 'NONE',  ( -1.813125098999968543, -7.427867185880000278, -434.7536662776001322 ) ) ;
#9622 = APPLICATION_PROTOCOL_DEFINITION ( 'draft international standard', 'automotive_design', 1998, #1109 ) ;
#9623 = LINE ( 'NONE', #1514, #8055 ) ;
#9624 = CYLINDRICAL_SURFACE ( 'NONE', #6610, 3.500000000000020428 ) ;
#9625 = EDGE_CURVE ( 'NONE', #10492, #7240, #10037, .T. ) ;
#9626 = CARTESIAN_POINT ( 'NONE',  ( -0.3140675329811673522, -12.00000000000000000, -361.6501536237392429 ) ) ;
#9627 = CARTESIAN_POINT ( 'NONE',  ( -16.76867785761999485, 5.202124494729996940, 319.9928079742500131 ) ) ;
#9628 = CARTESIAN_POINT ( 'NONE',  ( -1.301874420428522861, -2.640235564664999757, -434.9315895259924218 ) ) ;
#9629 = ORIENTED_EDGE ( 'NONE', *, *, #3001, .F. ) ;
#9630 = CARTESIAN_POINT ( 'NONE',  ( -20.05670149355997722, -0.5623089763428000820, -317.0792622552969533 ) ) ;
#9631 = CARTESIAN_POINT ( 'NONE',  ( -14.37110465573396212, -2.500000000000000000, -348.9812360766022721 ) ) ;
#9632 = AXIS2_PLACEMENT_3D ( 'NONE', #6245, #3889, #5383 ) ;
#9633 = APPLICATION_CONTEXT ( 'automotive_design' ) ;
#9634 = VERTEX_POINT ( 'NONE', #93 ) ;
#9635 = CARTESIAN_POINT ( 'NONE',  ( -2.000000000003786749, -9.500000000000001776, -409.4999999999758415 ) ) ;
#9636 = EDGE_CURVE ( 'NONE', #135, #9105, #6977, .T. ) ;
#9637 = LINE ( 'NONE', #8995, #511 ) ;
#9638 = DIRECTION ( 'NONE',  ( 0.000000000000000000, -1.000000000000000000, 0.000000000000000000 ) ) ;
#9639 = VERTEX_POINT ( 'NONE', #10182 ) ;
#9640 = CARTESIAN_POINT ( 'NONE',  ( -17.50000000000000000, 0.000000000000000000, -314.4999343908002061 ) ) ;
#9641 = VERTEX_POINT ( 'NONE', #1310 ) ;
#9642 = CARTESIAN_POINT ( 'NONE',  ( 19.99999036626000048, 4.642009117057000143E-09, -316.5000000000000000 ) ) ;
#9643 = ORIENTED_EDGE ( 'NONE', *, *, #9251, .T. ) ;
#9644 = CARTESIAN_POINT ( 'NONE',  ( -15.45559681510979466, -3.931366100772827998, 315.0000000000000000 ) ) ;
#9645 = CARTESIAN_POINT ( 'NONE',  ( -5.268482393219001025, -12.14948647186998976, -302.9207377450070453 ) ) ;
#9646 = FACE_OUTER_BOUND ( 'NONE', #10180, .T. ) ;
#9647 = CIRCLE ( 'NONE', #10324, 3.500000000000003109 ) ;
#9648 = CARTESIAN_POINT ( 'NONE',  ( 6.704579698891996564, 11.86746000475999452, -302.9207377450070453 ) ) ;
#9649 = ADVANCED_FACE ( 'NONE', ( #10240, #1102 ), #7662, .T. ) ;
#9650 = PRODUCT_DEFINITION_SHAPE ( 'NONE', 'NONE',  #10630 ) ;
#9651 = DIRECTION ( 'NONE',  ( 0.000000000000000000, 1.000000000000000000, 0.000000000000000000 ) ) ;
#9652 = VERTEX_POINT ( 'NONE', #10130 ) ;
#9653 = CARTESIAN_POINT ( 'NONE',  ( 12.17979804859000126, -7.053762231097000068, -314.6383426456000052 ) ) ;
#9654 = CARTESIAN_POINT ( 'NONE',  ( -14.37110465573396212, -7.500000000000000000, -348.9812360766022721 ) ) ;
#9655 = AXIS2_PLACEMENT_3D ( 'NONE', #2373, #2318, #9841 ) ;
#9656 = ORIENTED_EDGE ( 'NONE', *, *, #1217, .F. ) ;
#9657 = CARTESIAN_POINT ( 'NONE',  ( -15.34534221234999585, -7.499749350177997265, 189.9229057364800042 ) ) ;
#9658 = CARTESIAN_POINT ( 'NONE',  ( 7.561138155138405814, 11.58431960382585579, 190.9999999999996589 ) ) ;
#9659 = PLANE ( 'NONE',  #4135 ) ;
#9660 = CARTESIAN_POINT ( 'NONE',  ( -17.16710485141000220, -2.239552065056999997, 314.4150829855000211 ) ) ;
#9661 = FILL_AREA_STYLE ('',( #3104 ) ) ;
#9662 = CARTESIAN_POINT ( 'NONE',  ( -18.53283357168000123, 2.549981878952999992, 320.0000000000000000 ) ) ;
#9663 = CARTESIAN_POINT ( 'NONE',  ( 8.447271450478007537, -10.17170359172999738, 319.9928079742500131 ) ) ;
#9664 = CARTESIAN_POINT ( 'NONE',  ( 6.473926368715493318, 11.84005611832666460, 319.0000000000005116 ) ) ;
#9665 =( LENGTH_UNIT ( ) NAMED_UNIT ( * ) SI_UNIT ( .MILLI., .METRE. ) );
#9666 = FACE_OUTER_BOUND ( 'NONE', #9083, .T. ) ;
#9667 = ORIENTED_EDGE ( 'NONE', *, *, #1338, .T. ) ;
#9668 = CARTESIAN_POINT ( 'NONE',  ( 9.378959784071181360, -4.100000000000000533, -525.1866552614185366 ) ) ;
#9669 = VECTOR ( 'NONE', #9538, 1000.000000000000000 ) ;
#9670 = CARTESIAN_POINT ( 'NONE',  ( -17.30294281340998452, 5.653404495199006341, 189.9229057364800042 ) ) ;
#9671 = CARTESIAN_POINT ( 'NONE',  ( 10.23467949917770525, 9.999999999493887515, 190.0000000000002842 ) ) ;
#9672 = ORIENTED_EDGE ( 'NONE', *, *, #5752, .T. ) ;
#9673 = DIRECTION ( 'NONE',  ( -0.2951854283187965167, 0.000000000000000000, 0.9554399839384203341 ) ) ;
#9674 = CARTESIAN_POINT ( 'NONE',  ( 16.53777229716873265, 2.187293290751350483, 315.0000000000000000 ) ) ;
#9675 =( GEOMETRIC_REPRESENTATION_CONTEXT ( 3 ) GLOBAL_UNCERTAINTY_ASSIGNED_CONTEXT ( ( #772 ) ) GLOBAL_UNIT_ASSIGNED_CONTEXT ( ( #971, #4257, #7685 ) ) REPRESENTATION_CONTEXT ( 'NONE', 'WORKASPACE' ) );
#9676 = PRODUCT_CONTEXT ( 'NONE', #4147, 'mechanical' ) ;
#9677 = CARTESIAN_POINT ( 'NONE',  ( 5.046018101664359712, -12.10925368423180259, -303.4999999999996589 ) ) ;
#9678 = DIRECTION ( 'NONE',  ( 0.000000000000000000, -1.000000000000000000, 0.000000000000000000 ) ) ;
#9679 = CARTESIAN_POINT ( 'NONE',  ( -18.02719435607597021, -9.000000000000001776, -431.8467903975401896 ) ) ;
#9680 = B_SPLINE_CURVE_WITH_KNOTS ( 'NONE', 3,
 ( #183, #6739, #2653, #1845, #4090, #3980, #2263, #8174, #4684, #5638, #6507, #7959, #3280 ),
 .UNSPECIFIED., .F., .F.,
 ( 4, 1, 1, 1, 1, 1, 1, 1, 1, 1, 4 ),
 ( 0.000000000000000000, 0.08333333333333001192, 0.1666666666667000196, 0.2500000000000000000, 0.3333333333333000081, 0.5000000000000000000, 0.6666666666667000474, 0.7500000000000000000, 0.8333333333333000637, 0.9166666666667000474, 1.000000000000000000 ),
 .UNSPECIFIED. ) ;
#9681 = CARTESIAN_POINT ( 'NONE',  ( -17.27957593929000879, 4.562754682971998932, 319.9928079742500131 ) ) ;
#9682 = CIRCLE ( 'NONE', #414, 1.000000000000008882 ) ;
#9683 = CARTESIAN_POINT ( 'NONE',  ( -0.5535498271043974849, -7.499999952522999891, -434.2938920418101816 ) ) ;
#9684 = FACE_OUTER_BOUND ( 'NONE', #5453, .T. ) ;
#9685 = ORIENTED_EDGE ( 'NONE', *, *, #2068, .F. ) ;
#9686 = CARTESIAN_POINT ( 'NONE',  ( 19.57077664853002119, -0.3812814288523002082, -317.5770954168139610 ) ) ;
#9687 = DIRECTION ( 'NONE',  ( -0.9627070496199739980, 0.1321637200910051047, -0.2360675490272045873 ) ) ;
#9688 = TOROIDAL_SURFACE ( 'NONE', #10544, 12.50000000000000000, 0.5000000000000000000 ) ;
#9689 = AXIS2_PLACEMENT_3D ( 'NONE', #7947, #6441, #10468 ) ;
#9690 = EDGE_CURVE ( 'NONE', #9423, #10046, #2835, .T. ) ;
#9691 = CARTESIAN_POINT ( 'NONE',  ( 0.000000000000000000, 0.000000000000000000, -317.5000000000000000 ) ) ;
#9692 = LINE ( 'NONE', #3354, #169 ) ;
#9693 = DIRECTION ( 'NONE',  ( 0.000000000000000000, -1.000000000000000000, 0.000000000000000000 ) ) ;
#9694 = VECTOR ( 'NONE', #2511, 1000.000000000000000 ) ;
#9696 = ORIENTED_EDGE ( 'NONE', *, *, #8175, .F. ) ;
#9695 =( GEOMETRIC_REPRESENTATION_CONTEXT ( 3 ) GLOBAL_UNCERTAINTY_ASSIGNED_CONTEXT ( ( #1634 ) ) GLOBAL_UNIT_ASSIGNED_CONTEXT ( ( #4296, #5787, #903 ) ) REPRESENTATION_CONTEXT ( 'NONE', 'WORKASPACE' ) );
#9697 = CYLINDRICAL_SURFACE ( 'NONE', #4183, 19.99999999999998934 ) ;
#9698 = ORIENTED_EDGE ( 'NONE', *, *, #5141, .F. ) ;
#9699 = CARTESIAN_POINT ( 'NONE',  ( 9.195128512800469167, 11.11313767369120953, -316.5000000000004547 ) ) ;
#9700 = ORIENTED_EDGE ( 'NONE', *, *, #833, .F. ) ;
#9701 = CARTESIAN_POINT ( 'NONE',  ( -8.021995032228604217, -8.375907102466543463, 315.0000000000000568 ) ) ;
#9702 = CARTESIAN_POINT ( 'NONE',  ( -1.988818824435997890, -12.53224469152999099, -302.9207377450070453 ) ) ;
#9703 = EDGE_CURVE ( 'NONE', #6862, #3094, #3731, .T. ) ;
#9704 = CARTESIAN_POINT ( 'NONE',  ( -46.74071243419621169, -9.500000000000001776, -414.3237589990241077 ) ) ;
#9705 = ADVANCED_FACE ( 'NONE', ( #8608 ), #1968, .T. ) ;
#9706 = DIRECTION ( 'NONE',  ( -0.1071946444232958900, 0.000000000000000000, 0.9942380540931649024 ) ) ;
#9707 =( GEOMETRIC_REPRESENTATION_CONTEXT ( 3 ) GLOBAL_UNCERTAINTY_ASSIGNED_CONTEXT ( ( #2278 ) ) GLOBAL_UNIT_ASSIGNED_CONTEXT ( ( #10040, #9342, #2682 ) ) REPRESENTATION_CONTEXT ( 'NONE', 'WORKASPACE' ) );
#9708 = CARTESIAN_POINT ( 'NONE',  ( 13.92883798546999508, 9.075834183867002025, -302.9207377450070453 ) ) ;
#9709 = CARTESIAN_POINT ( 'NONE',  ( 19.77468550638000266, -1.920668048511998904, 318.8802828394900644 ) ) ;
#9710 = VERTEX_POINT ( 'NONE', #2826 ) ;
#9711 = CARTESIAN_POINT ( 'NONE',  ( -11.99990625867999938, -6.898016740823000426, -314.8616023057000461 ) ) ;
#9712 = DIRECTION ( 'NONE',  ( 0.000000000000000000, 1.000000000000000000, -0.000000000000000000 ) ) ;
#9713 = ORIENTED_EDGE ( 'NONE', *, *, #2673, .T. ) ;
#9714 = CARTESIAN_POINT ( 'NONE',  ( -18.45932313982999062, -2.405278989253002209, 190.0071920248299477 ) ) ;
#9715 = CARTESIAN_POINT ( 'NONE',  ( -4.856005603318366504, 12.14126555804866570, 190.9999999999996589 ) ) ;
#9716 = CARTESIAN_POINT ( 'NONE',  ( -0.6600669447125837586, -8.000000000000000000, -421.9279756761403632 ) ) ;
#9717 = PRODUCT_DEFINITION_FORMATION_WITH_SPECIFIED_SOURCE ( 'ANY', '', #381, .NOT_KNOWN. ) ;
#9718 = EDGE_CURVE ( 'NONE', #8716, #7492, #601, .T. ) ;
#9719 = CARTESIAN_POINT ( 'NONE',  ( -3.846123575835999731, -9.203727088275000412, 315.0848619657999734 ) ) ;
#9720 = DIRECTION ( 'NONE',  ( -1.000000000000000000, 0.000000000000000000, 0.000000000000000000 ) ) ;
#9721 = LINE ( 'NONE', #2466, #4850 ) ;
#9722 = CARTESIAN_POINT ( 'NONE',  ( -18.14104367554000774, -3.149620910056999623, 319.9928079742500131 ) ) ;
#9723 = DIRECTION ( 'NONE',  ( 0.7220286942758216142, 0.000000000000000000, 0.6918631112021741414 ) ) ;
#9724 = FILL_AREA_STYLE ('',( #8971 ) ) ;
#9725 = CARTESIAN_POINT ( 'NONE',  ( 16.99996037728000076, -1.352915776343000118E-09, 314.9999801883000146 ) ) ;
#9726 = EDGE_LOOP ( 'NONE', ( #6430, #873, #7420, #9433 ) ) ;
#9727 = CARTESIAN_POINT ( 'NONE',  ( 0.000000000000000000, 7.937240849781000307, -285.0000000000000000 ) ) ;
#9728 = CARTESIAN_POINT ( 'NONE',  ( 17.32898823752001860, 5.623515075799002894, 189.9229057364800042 ) ) ;
#9729 = FACE_OUTER_BOUND ( 'NONE', #7063, .T. ) ;
#9730 = FACE_BOUND ( 'NONE', #5826, .T. ) ;
#9731 = CARTESIAN_POINT ( 'NONE',  ( 13.97618761079829142, 5.383201530108604693, 314.9999999999999432 ) ) ;
#9732 = CARTESIAN_POINT ( 'NONE',  ( 19.86889125890001040, -1.746333262808030584, -303.5000000000005684 ) ) ;
#9733 = CARTESIAN_POINT ( 'NONE',  ( 17.35477687787999912, -0.3068793820639000303, -314.6383426456000052 ) ) ;
#9734 = DIRECTION ( 'NONE',  ( -0.2951854283188045658, 0.000000000000000000, 0.9554399839384177806 ) ) ;
#9735 = DIRECTION ( 'NONE',  ( 0.4716280258120408853, 0.000000000000000000, -0.8817975988108818219 ) ) ;
#9736 = CARTESIAN_POINT ( 'NONE',  ( -17.73249602794001234, 3.891729847315997581, 319.9928079742500131 ) ) ;
#9737 = CARTESIAN_POINT ( 'NONE',  ( -83.90876261087991850, -2.500000000000000000, -346.8809236044617137 ) ) ;
#9738 = CARTESIAN_POINT ( 'NONE',  ( -1.071307256257647333, -2.585569669607997945, -434.6046133433468412 ) ) ;
#9739 = ORIENTED_EDGE ( 'NONE', *, *, #2673, .F. ) ;
#9740 = CARTESIAN_POINT ( 'NONE',  ( 17.71107981743001503, 5.830323931021004213, -316.3802825947000201 ) ) ;
#9741 = CARTESIAN_POINT ( 'NONE',  ( -98.44423576012317767, -2.500000000000000000, -338.7741350709160315 ) ) ;
#9742 = EDGE_CURVE ( 'NONE', #6040, #4813, #7811, .T. ) ;
#9743 = ORIENTED_EDGE ( 'NONE', *, *, #6736, .T. ) ;
#9744 = CARTESIAN_POINT ( 'NONE',  ( 14.17215049938999982, -7.636433089049000422, 320.0000000000000000 ) ) ;
#9745 = CARTESIAN_POINT ( 'NONE',  ( -0.3590672782033171861, -7.540140950748998705, -433.9280555215146364 ) ) ;
#9746 = CIRCLE ( 'NONE', #4079, 5.000000000000004441 ) ;
#9747 = CARTESIAN_POINT ( 'NONE',  ( -14.00000000000000000, -2.500000000000000000, -317.5000000000000000 ) ) ;
#9748 = CARTESIAN_POINT ( 'NONE',  ( -17.50000000000000000, 0.000000000000000000, -314.4999343908002061 ) ) ;
#9749 = ORIENTED_EDGE ( 'NONE', *, *, #4906, .T. ) ;
#9750 = CARTESIAN_POINT ( 'NONE',  ( -17.27223423031420069, -1.573973318776765717, -314.5135302205611083 ) ) ;
#9751 = EDGE_LOOP ( 'NONE', ( #6982, #2689, #751, #3674 ) ) ;
#9752 = CARTESIAN_POINT ( 'NONE',  ( -10.59678593799237944, 10.61334907845371411, -316.5000000000004547 ) ) ;
#9753 = ORIENTED_EDGE ( 'NONE', *, *, #2451, .T. ) ;
#9754 = CARTESIAN_POINT ( 'NONE',  ( 0.3943348293965602824, -9.499921225251823031, 315.0000000000000000 ) ) ;
#9755 = CARTESIAN_POINT ( 'NONE',  ( -12.62193639354000396, -9.236300292413996971, -302.4229045757450081 ) ) ;
#9756 = EDGE_CURVE ( 'NONE', #8275, #3792, #6097, .T. ) ;
#9757 = CARTESIAN_POINT ( 'NONE',  ( -2.000000000003786749, -9.000000000000001776, -409.4999999999758415 ) ) ;
#9758 = DIRECTION ( 'NONE',  ( -0.2381566831044910626, 0.000000000000000000, 0.9712267471052612455 ) ) ;
#9759 =( NAMED_UNIT ( * ) PLANE_ANGLE_UNIT ( ) SI_UNIT ( $, .RADIAN. ) );
#9760 = CARTESIAN_POINT ( 'NONE',  ( 18.60584266697000544, 4.788593885995998889, -302.9207377450070453 ) ) ;
#9761 = CARTESIAN_POINT ( 'NONE',  ( 19.12221666159999600, -3.679580603257996962, 318.8802828394900644 ) ) ;
#9762 = ORIENTED_EDGE ( 'NONE', *, *, #10296, .T. ) ;
#9763 = CARTESIAN_POINT ( 'NONE',  ( 1.419551022038999966, -10.09154694854999867, -314.4150829855000211 ) ) ;
#9764 = EDGE_CURVE ( 'NONE', #9430, #4467, #7018, .T. ) ;
#9765 = CARTESIAN_POINT ( 'NONE',  ( -14.00000000000000000, -2.500000000000000000, -380.4979246178999688 ) ) ;
#9766 = VERTEX_POINT ( 'NONE', #3581 ) ;
#9767 = CARTESIAN_POINT ( 'NONE',  ( 19.59090808375999515, -0.09664295149309998223, 189.9229057364800042 ) ) ;
#9768 = CARTESIAN_POINT ( 'NONE',  ( 19.96251415050937439, 0.9422375983257499366, 190.9999999999996589 ) ) ;
#9769 = CARTESIAN_POINT ( 'NONE',  ( -0.7884827272773663465, 9.499887003984509803, -315.0000000000000568 ) ) ;
#9770 = LINE ( 'NONE', #2408, #8245 ) ;
#9771 = CARTESIAN_POINT ( 'NONE',  ( 4.031301020048999817, -9.630010295875997883, 314.6383426456000052 ) ) ;
#9772 =( NAMED_UNIT ( * ) SI_UNIT ( $, .STERADIAN. ) SOLID_ANGLE_UNIT ( ) );
#9773 = CARTESIAN_POINT ( 'NONE',  ( -7.333949653644999955, 10.60950709473999964, 320.0000000000000000 ) ) ;
#9774 = CARTESIAN_POINT ( 'NONE',  ( 10.54676984209158519, -2.500000000000000000, -347.8422498368975084 ) ) ;
#9775 = CARTESIAN_POINT ( 'NONE',  ( 15.66137281426500572, 7.786477173011509656, 319.0000000000005116 ) ) ;
#9776 = CARTESIAN_POINT ( 'NONE',  ( -1.514431797236434930E-09, -10.00000000000000000, 190.0000000000000000 ) ) ;
#9777 = CARTESIAN_POINT ( 'NONE',  ( -18.02719435607597021, -8.000000000000000000, -431.8467903975401896 ) ) ;
#9778 = ORIENTED_EDGE ( 'NONE', *, *, #9983, .T. ) ;
#9779 = LINE ( 'NONE', #7311, #6202 ) ;
#9780 = ORIENTED_EDGE ( 'NONE', *, *, #3202, .F. ) ;
#9781 = CIRCLE ( 'NONE', #1361, 4.000000000000009770 ) ;
#9782 = VECTOR ( 'NONE', #8933, 1000.000000000000000 ) ;
#9783 = ORIENTED_EDGE ( 'NONE', *, *, #1933, .T. ) ;
#9784 = CARTESIAN_POINT ( 'NONE',  ( 20.00000000435078107, -7.322330466941333604, -316.5000000000000000 ) ) ;
#9785 = CIRCLE ( 'NONE', #2409, 4.000000000000000000 ) ;
#9786 = CARTESIAN_POINT ( 'NONE',  ( 16.99953299605537183, 0.4334412736564768331, 315.0000000000000568 ) ) ;
#9787 = DIRECTION ( 'NONE',  ( 0.5469441386039884945, -8.342642289485093768E-17, -0.8371691043312222691 ) ) ;
#9788 = CARTESIAN_POINT ( 'NONE',  ( 19.32402384659099326, -3.348155292981250586, -303.4999999999996589 ) ) ;
#9789 = CARTESIAN_POINT ( 'NONE',  ( -13.34617449956999913, -8.168334506422000985, -302.5000000000000000 ) ) ;
#9790 = DIRECTION ( 'NONE',  ( -0.1173809667161559989, 0.000000000000000000, 0.9930869592602555862 ) ) ;
#9791 = DIRECTION ( 'NONE',  ( 0.7172627762233165782, 0.1147078669353000374, 0.6872963080852203532 ) ) ;
#9792 = CARTESIAN_POINT ( 'NONE',  ( 19.86662547467000550, 1.900306748470001139, 319.5792614743400009 ) ) ;
#9793 = LINE ( 'NONE', #1572, #9127 ) ;
#9794 = CARTESIAN_POINT ( 'NONE',  ( -0.7127201389310124924, -2.500198451567999580, -434.8920403824821506 ) ) ;
#9795 = CARTESIAN_POINT ( 'NONE',  ( 1.525345003100600394, -7.500000000000000000, -348.4143162901089568 ) ) ;
#9796 = CARTESIAN_POINT ( 'NONE',  ( -6.751314262718001835, 11.77064546103999731, -316.3802825947000201 ) ) ;
#9797 = VECTOR ( 'NONE', #4722, 1000.000000000000000 ) ;
#9798 = CARTESIAN_POINT ( 'NONE',  ( -11.66516470684000772, -10.15894662545001381, -316.3802825947000201 ) ) ;
#9799 = ORIENTED_EDGE ( 'NONE', *, *, #6343, .F. ) ;
#9800 = CARTESIAN_POINT ( 'NONE',  ( -16.29068328802999943, -5.892689959824000567, 320.0000000000000000 ) ) ;
#9801 = CARTESIAN_POINT ( 'NONE',  ( -0.7425212270488497079, -7.493595516397002498, -434.9074498605589838 ) ) ;
#9802 = CARTESIAN_POINT ( 'NONE',  ( -41.41721991556968874, -12.50000000000000000, -366.3159076589344636 ) ) ;
#9803 = CARTESIAN_POINT ( 'NONE',  ( 8.778856717165009371, -8.123403389731517876, -315.0000000000001137 ) ) ;
#9804 = ORIENTED_EDGE ( 'NONE', *, *, #5800, .T. ) ;
#9805 = CARTESIAN_POINT ( 'NONE',  ( -15.67978886374999803, 4.575336738469999887, -314.4963898845653603 ) ) ;
#9806 = VERTEX_POINT ( 'NONE', #7864 ) ;
#9807 = DIRECTION ( 'NONE',  ( 0.000000000000000000, -1.000000000000000000, 0.000000000000000000 ) ) ;
#9808 = ORIENTED_EDGE ( 'NONE', *, *, #7155, .T. ) ;
#9809 = CARTESIAN_POINT ( 'NONE',  ( 17.74191744551998795, -5.793625128177000150, -303.6197174156509391 ) ) ;
#9810 = CARTESIAN_POINT ( 'NONE',  ( -87.43749534091338660, -2.500000000000000000, -367.8627987905216514 ) ) ;
#9811 = CARTESIAN_POINT ( 'NONE',  ( -13.57573464316000056, -3.225916527208000151, 315.0000000000000000 ) ) ;
#9812 = CARTESIAN_POINT ( 'NONE',  ( -19.56988197685000230, -0.3940236285954000772, -302.4229045757450081 ) ) ;
#9813 = CARTESIAN_POINT ( 'NONE',  ( 19.00000000000000000, 0.000000000000000000, -302.5000000001010108 ) ) ;
#9814 = ORIENTED_EDGE ( 'NONE', *, *, #8963, .T. ) ;
#9815 = CARTESIAN_POINT ( 'NONE',  ( -16.89608781496000134, -0.5923740909019999945, -315.0848619657999734 ) ) ;
#9816 = CARTESIAN_POINT ( 'NONE',  ( -11.28854116844999922, 9.238965579841000419, -302.5000000000000000 ) ) ;
#9817 = ORIENTED_EDGE ( 'NONE', *, *, #1995, .F. ) ;
#9818 = CIRCLE ( 'NONE', #4839, 12.50000000000000178 ) ;
#9819 = CARTESIAN_POINT ( 'NONE',  ( -17.86997157320001151, -4.940892756443005851, 189.9229057364800042 ) ) ;
#9820 = DIRECTION ( 'NONE',  ( 0.000000000000000000, 0.7071067811864846231, 0.7071067811866105224 ) ) ;
#9821 = CARTESIAN_POINT ( 'NONE',  ( 10.90988923471839023, 7.272053090123300478, -315.0000000000000000 ) ) ;
#9822 = DIRECTION ( 'NONE',  ( 0.000000000000000000, -1.000000000000000000, -0.000000000000000000 ) ) ;
#9823 = EDGE_CURVE ( 'NONE', #4605, #5301, #8146, .T. ) ;
#9824 = CIRCLE ( 'NONE', #6738, 12.50000000000002487 ) ;
#9825 = CARTESIAN_POINT ( 'NONE',  ( -11.99990625867999938, -6.898016740823000426, 314.8616023057000461 ) ) ;
#9826 = EDGE_CURVE ( 'NONE', #9710, #4191, #10371, .T. ) ;
#9827 = CARTESIAN_POINT ( 'NONE',  ( -18.99998145310000197, 0.3132853329045000024, 319.9999999999899956 ) ) ;
#9828 = AXIS2_PLACEMENT_3D ( 'NONE', #3322, #1872, #6767 ) ;
#9829 = CARTESIAN_POINT ( 'NONE',  ( 17.73249602794001234, -3.891729847315997581, 319.9928079742500131 ) ) ;
#9830 = CARTESIAN_POINT ( 'NONE',  ( -19.78167965760190938, 1.922413304792618405, 319.0000000000005116 ) ) ;
#9831 = FILL_AREA_STYLE_COLOUR ( '', #3176 ) ;
#9832 = DIRECTION ( 'NONE',  ( 0.2951854283188049544, 0.000000000000000000, -0.9554399839384174475 ) ) ;
#9833 = EDGE_LOOP ( 'NONE', ( #9974, #6303, #10243, #4758 ) ) ;
#9834 = CARTESIAN_POINT ( 'NONE',  ( -11.28781796570999951, 4.951468039558000633, -285.0000000000000000 ) ) ;
#9835 = ORIENTED_EDGE ( 'NONE', *, *, #8771, .F. ) ;
#9836 = EDGE_CURVE ( 'NONE', #6747, #563, #2980, .T. ) ;
#9837 = VECTOR ( 'NONE', #8421, 1000.000000000000000 ) ;
#9838 = ADVANCED_FACE ( 'NONE', ( #2227 ), #6251, .T. ) ;
#9839 = CARTESIAN_POINT ( 'NONE',  ( -15.16362200326591569, -6.750000000000000000, -437.6963039377973246 ) ) ;
#9840 =( BOUNDED_CURVE ( )  B_SPLINE_CURVE ( 3, ( #7839, #9409, #538, #1996, #7737, #487, #9457 ),
 .UNSPECIFIED., .F., .T. ) 
 B_SPLINE_CURVE_WITH_KNOTS ( ( 4, 3, 4 ),
 ( 0.006576891535901297804, 0.5000000000000000000, 0.9934231084340220397 ),
 .UNSPECIFIED. ) 
 CURVE ( )  GEOMETRIC_REPRESENTATION_ITEM ( )  RATIONAL_B_SPLINE_CURVE ( ( 0.9922222088160741471, 0.8003084355042745512, 0.8029010325655832059, 1.000000000000000000, 0.8029010325775973733, 0.8003084355045906317, 0.9922222087809797753 ) ) 
 REPRESENTATION_ITEM ( '' )  );
#9841 = DIRECTION ( 'NONE',  ( 0.9902680687415800209, 0.000000000000000000, 0.1391731009599966873 ) ) ;
#9842 = CARTESIAN_POINT ( 'NONE',  ( 13.93992802816216781, -8.979094264391768832, -303.4999999999996589 ) ) ;
#9843 = CARTESIAN_POINT ( 'NONE',  ( 15.89383674730000173, 3.622219875512000087, -314.8616023057000461 ) ) ;
#9844 = APPLICATION_CONTEXT ( 'automotive_design' ) ;
#9845 = CARTESIAN_POINT ( 'NONE',  ( -18.53285823922000120, 2.549737172213000225, 190.0000000000000000 ) ) ;
#9846 = CARTESIAN_POINT ( 'NONE',  ( -14.89424055888783727, -5.714488051281095160, -438.7948683809335080 ) ) ;
#9847 = CARTESIAN_POINT ( 'NONE',  ( -13.57573464316000056, 3.225916527208000151, 315.0000000000001705 ) ) ;
#9848 = ORIENTED_EDGE ( 'NONE', *, *, #113, .F. ) ;
#9849 = CARTESIAN_POINT ( 'NONE',  ( 18.60752753902997725, 4.785892219302998463, -317.0792622552969533 ) ) ;
#9850 = DIRECTION ( 'NONE',  ( -0.9396926207858972147, 0.000000000000000000, -0.3420201433256990775 ) ) ;
#9851 = ADVANCED_FACE ( 'NONE', ( #5441 ), #9697, .F. ) ;
#9852 = PRESENTATION_LAYER_ASSIGNMENT (  '', '', ( #6938 ) ) ;
#9853 = CARTESIAN_POINT ( 'NONE',  ( -18.95677580539999951, -0.9180370088860999589, 320.0000000000000000 ) ) ;
#9854 = VECTOR ( 'NONE', #2234, 1000.000000000000000 ) ;
#9855 = CARTESIAN_POINT ( 'NONE',  ( -0.7911908081797823789, -7.435692558170999611, -434.7046119063388119 ) ) ;
#9856 = CARTESIAN_POINT ( 'NONE',  ( -81.08127826530241578, -7.500000000000000000, -352.1729300552810855 ) ) ;
#9857 = CARTESIAN_POINT ( 'NONE',  ( 3.689485142014392149, -9.275849510248951546, -314.9999999999999432 ) ) ;
#9858 = ORIENTED_EDGE ( 'NONE', *, *, #554, .F. ) ;
#9859 = CARTESIAN_POINT ( 'NONE',  ( 9.847343584659233429, -8.231878686604515494, -314.5529121822860361 ) ) ;
#9860 = AXIS2_PLACEMENT_3D ( 'NONE', #9679, #4744, #9790 ) ;
#9861 = ORIENTED_EDGE ( 'NONE', *, *, #5460, .T. ) ;
#9862 = CARTESIAN_POINT ( 'NONE',  ( -14.34749558092999777, 7.521529436904000221, -317.5000000000000000 ) ) ;
#9863 = EDGE_LOOP ( 'NONE', ( #7439, #4272, #3460, #7862 ) ) ;
#9864 = CARTESIAN_POINT ( 'NONE',  ( 9.278531818924999897, -11.16715007748999078, -302.9207377450070453 ) ) ;
#9865 = CLOSED_SHELL ( 'NONE', ( #353, #2206, #5871, #10389, #4706, #7025, #1812, #101 ) ) ;
#9866 = CARTESIAN_POINT ( 'NONE',  ( 3.713744197507001576, -11.87335072286999527, -317.5770954168139610 ) ) ;
#9867 = CARTESIAN_POINT ( 'NONE',  ( -14.79012398733999945, -1.483731117707000058, 315.0000000000000000 ) ) ;
#9868 = VECTOR ( 'NONE', #9420, 1000.000000000000000 ) ;
#9869 = AXIS2_PLACEMENT_3D ( 'NONE', #2717, #5232, #4383 ) ;
#9870 = CARTESIAN_POINT ( 'NONE',  ( -19.95943119690998557, 1.720147047185998757, -302.9207377450070453 ) ) ;
#9871 = CARTESIAN_POINT ( 'NONE',  ( -17.50000000000000000, 1.896400240175167841E-08, 314.4999014931028682 ) ) ;
#9872 = ORIENTED_EDGE ( 'NONE', *, *, #8432, .F. ) ;
#9873 = CARTESIAN_POINT ( 'NONE',  ( -17.56970546055000071, 0.4338786413876999926, -314.4150829855000211 ) ) ;
#9874 = DIRECTION ( 'NONE',  ( -0.9712267471052612455, 0.000000000000000000, -0.2381566831044910626 ) ) ;
#9875 = EDGE_LOOP ( 'NONE', ( #9753, #3732, #7441, #5444, #9743, #1770, #3327, #622 ) ) ;
#9876 = CARTESIAN_POINT ( 'NONE',  ( -18.27235334878999851, -5.234940180598000481, 190.4207385301700128 ) ) ;
#9877 = CARTESIAN_POINT ( 'NONE',  ( -8.037373804805000077, -9.179324345868998591, -314.4944826805095772 ) ) ;
#9878 = CARTESIAN_POINT ( 'NONE',  ( 11.54764063961475351, 6.952680983979389495, -315.0000000000000000 ) ) ;
#9879 = DIRECTION ( 'NONE',  ( 0.1071946444232954182, 0.000000000000000000, -0.9942380540931651245 ) ) ;
#9880 = EDGE_CURVE ( 'NONE', #4852, #9887, #6468, .T. ) ;
#9881 = CARTESIAN_POINT ( 'NONE',  ( 8.551447359560999217, -8.144527334518999240, 315.0848619657999734 ) ) ;
#9882 = B_SPLINE_CURVE_WITH_KNOTS ( 'NONE', 3,
 ( #6518, #9046, #9853, #769, #718, #1681, #8076, #1472, #1632, #9800, #3352, #820, #4051, #70, #2437, #6570, #6627, #8022, #4905, #3991, #8184, #3241, #7380, #6409, #4154, #2275, #15, #3289, #1522, #2492, #4955, #7222, #10489, #10548, #3190, #9744, #6462, #5650, #8231, #868, #1579, #4856, #9956, #6792, #10064, #8283, #6735, #7640 ),
 .UNSPECIFIED., .F., .F.,
 ( 4, 1, 1, 1, 1, 1, 1, 1, 1, 1, 1, 1, 1, 1, 1, 1, 1, 1, 1, 1, 1, 1, 1, 1, 1, 1, 1, 1, 1, 1, 1, 1, 1, 1, 1, 1, 1, 1, 1, 1, 1, 1, 1, 1, 1, 4 ),
 ( 0.000000000000000000, 0.02222222222221999915, 0.04444444444443999831, 0.06666666666666999641, 0.08888888888889000250, 0.1111111111111000027, 0.1333333333332999970, 0.1555555555555999947, 0.1777777777777999890, 0.2000000000000000111, 0.2222222222222000054, 0.2444444444443999997, 0.2666666666666999697, 0.2888888888889000195, 0.3111111111111000138, 0.3333333333333000081, 0.3555555555556000336, 0.3777777777777999724, 0.4000000000000000222, 0.4222222222221999610, 0.4444444444444000109, 0.4666666666666999808, 0.4888888888889000306, 0.5111111111110999694, 0.5333333333333000192, 0.5555555555555999891, 0.5777777777778000390, 0.5999999999999999778, 0.6222222222222000276, 0.6444444444443999664, 0.6666666666667000474, 0.6888888888888999862, 0.7111111111111000360, 0.7333333333333000859, 0.7555555555556000558, 0.7777777777777999946, 0.8000000000000000444, 0.8222222222221999832, 0.8444444444443999220, 0.8666666666667000030, 0.8888888888888999418, 0.9111111111110999916, 0.9333333333333000414, 0.9555555555556000114, 0.9777777777778000612, 1.000000000000000000 ),
 .UNSPECIFIED. ) ;
#9883 = CARTESIAN_POINT ( 'NONE',  ( -86.86306229143158930, -7.500000000000000000, -370.6132103076870976 ) ) ;
#9884 = CARTESIAN_POINT ( 'NONE',  ( 18.75085780967000559, -3.496151560526002289, 320.0770942683900557 ) ) ;
#9885 = CARTESIAN_POINT ( 'NONE',  ( -7.495586483745387163, 11.60098025501653929, 319.0000000000005116 ) ) ;
#9886 = CARTESIAN_POINT ( 'NONE',  ( 15.89383674730000173, 3.622219875512000087, 314.8616023057000461 ) ) ;
#9887 = VERTEX_POINT ( 'NONE', #2337 ) ;
#9888 = CARTESIAN_POINT ( 'NONE',  ( 19.49681644515301215, -2.834072041603171499, 190.9999999999995737 ) ) ;
#9889 = VERTEX_POINT ( 'NONE', #7172 ) ;
#9890 = ORIENTED_EDGE ( 'NONE', *, *, #9368, .F. ) ;
#9891 = EDGE_CURVE ( 'NONE', #9921, #4804, #6189, .T. ) ;
#9892 = ADVANCED_FACE ( 'NONE', ( #2657 ), #21, .T. ) ;
#9893 = CARTESIAN_POINT ( 'NONE',  ( -2.852327370720492805, -2.558519736919000032, -435.0254095138128605 ) ) ;
#9894 = LINE ( 'NONE', #1435, #9797 ) ;
#9895 = CARTESIAN_POINT ( 'NONE',  ( -1.873948611771682149, -7.500000000000000888, -349.2478646809681777 ) ) ;
#9896 = CARTESIAN_POINT ( 'NONE',  ( -2.000000000000000000, -9.500000000000000000, -409.5000000000000000 ) ) ;
#9897 = ORIENTED_EDGE ( 'NONE', *, *, #4829, .T. ) ;
#9898 = DIRECTION ( 'NONE',  ( 0.000000000000000000, 1.000000000000000000, -0.000000000000000000 ) ) ;
#9899 = CARTESIAN_POINT ( 'NONE',  ( -14.24871951745999965, 7.583581010724000038, 190.0000000000000000 ) ) ;
#9900 = ADVANCED_FACE ( 'NONE', ( #9157 ), #3861, .T. ) ;
#9901 = CARTESIAN_POINT ( 'NONE',  ( -2.000000000000000000, 2.500000000000000000, -409.5000000000000568 ) ) ;
#9902 = CARTESIAN_POINT ( 'NONE',  ( 15.00000000000325784, -8.632726818195413123E-17, 315.0000000000001705 ) ) ;
#9903 = CARTESIAN_POINT ( 'NONE',  ( -20.32733171007796713, -2.500000000000000000, -429.5091673395090766 ) ) ;
#9904 = CARTESIAN_POINT ( 'NONE',  ( -12.86351645698000645, 9.576920946250998767, -316.3802825947000201 ) ) ;
#9905 = FACE_BOUND ( 'NONE', #253, .T. ) ;
#9906 = CARTESIAN_POINT ( 'NONE',  ( -1.821036076062871656, -7.345996400954998506, -434.8999269110483397 ) ) ;
#9907 = DIRECTION ( 'NONE',  ( -0.9902680687415800209, 0.000000000000000000, -0.1391731009599965763 ) ) ;
#9908 = CARTESIAN_POINT ( 'NONE',  ( -0.9838506439437841866, -9.488399989288446079, -315.0000000000000000 ) ) ;
#9909 = ORIENTED_EDGE ( 'NONE', *, *, #1952, .T. ) ;
#9910 = CARTESIAN_POINT ( 'NONE',  ( 17.48550435259292612, -0.4594173590775665339, -314.5005290240521276 ) ) ;
#9911 = ORIENTED_EDGE ( 'NONE', *, *, #1668, .F. ) ;
#9912 = CARTESIAN_POINT ( 'NONE',  ( -14.00000000000000000, 2.500000000000000000, -380.4979246178999688 ) ) ;
#9913 = EDGE_LOOP ( 'NONE', ( #350, #675, #1637, #10146 ) ) ;
#9914 = CARTESIAN_POINT ( 'NONE',  ( 5.058393412147005108, -12.18538300202998315, -302.9207377450070453 ) ) ;
#9915 = FACE_OUTER_BOUND ( 'NONE', #3097, .T. ) ;
#9916 = DIRECTION ( 'NONE',  ( -0.1124491875265153235, 0.000000000000000000, 0.9936574763089273121 ) ) ;
#9917 = VECTOR ( 'NONE', #6932, 1000.000000000000000 ) ;
#9918 = CARTESIAN_POINT ( 'NONE',  ( -6.514701929829219473, -7.147380552937434572, -436.2336181546095872 ) ) ;
#9919 = CARTESIAN_POINT ( 'NONE',  ( -17.22664556233274880, -1.821222559103062633, 314.4999497328576012 ) ) ;
#9920 =( BOUNDED_CURVE ( )  B_SPLINE_CURVE ( 3, ( #1117, #2735, #7674, #1168 ),
 .UNSPECIFIED., .F., .T. ) 
 B_SPLINE_CURVE_WITH_KNOTS ( ( 4, 4 ),
 ( 1.073606735059035064E-09, 1.000000000000000000 ),
 .UNSPECIFIED. ) 
 CURVE ( )  GEOMETRIC_REPRESENTATION_ITEM ( )  RATIONAL_B_SPLINE_CURVE ( ( 0.9922222082322698089, 0.8003084355095323454, 0.8029010327654424461, 1.000000000000000000 ) ) 
 REPRESENTATION_ITEM ( '' )  );
#9921 = VERTEX_POINT ( 'NONE', #9216 ) ;
#9922 = CARTESIAN_POINT ( 'NONE',  ( -16.54291557298000370, -1.991497705781999805, -315.0848619657999734 ) ) ;
#9923 = DIRECTION ( 'NONE',  ( 0.8820010751365664481, 0.000000000000000000, 0.4712473909295847307 ) ) ;
#9924 = ORIENTED_EDGE ( 'NONE', *, *, #1668, .T. ) ;
#9925 = CARTESIAN_POINT ( 'NONE',  ( -11.06049270995999123, -10.50744457173999713, 190.4207385301700128 ) ) ;
#9926 = VECTOR ( 'NONE', #3588, 1000.000000000000000 ) ;
#9927 = LINE ( 'NONE', #204, #4700 ) ;
#9928 = DIRECTION ( 'NONE',  ( 1.477360691113388328E-12, 1.000000000000000000, 1.592829336162332234E-13 ) ) ;
#9929 = CARTESIAN_POINT ( 'NONE',  ( -14.74684780783305449, -4.500000000000000888, -439.3959507452315165 ) ) ;
#9930 = CARTESIAN_POINT ( 'NONE',  ( -19.49006540358000805, 2.831553480999998929, 191.1197171614399792 ) ) ;
#9931 = CARTESIAN_POINT ( 'NONE',  ( 14.43094748301999886, -5.211771040651000497, 314.8616023057000461 ) ) ;
#9932 = CYLINDRICAL_SURFACE ( 'NONE', #9828, 10.00000000000000000 ) ;
#9933 = CARTESIAN_POINT ( 'NONE',  ( -19.38188031595998595, -1.781951755297001450, 320.0770942683900557 ) ) ;
#9934 = DIRECTION ( 'NONE',  ( -0.4712473909295827323, 0.000000000000000000, 0.8820010751365675583 ) ) ;
#9935 = CARTESIAN_POINT ( 'NONE',  ( -6.533799827619673373, 11.82671337997188132, -303.5000000000000000 ) ) ;
#9936 = CARTESIAN_POINT ( 'NONE',  ( 6.370857846455999507, 9.209451711050000711, 314.6383426456000052 ) ) ;
#9937 = ORIENTED_EDGE ( 'NONE', *, *, #7909, .F. ) ;
#9938 = LINE ( 'NONE', #8375, #3641 ) ;
#9939 = ORIENTED_EDGE ( 'NONE', *, *, #8044, .T. ) ;
#9940 = ADVANCED_FACE ( 'NONE', ( #777 ), #2804, .F. ) ;
#9941 = CARTESIAN_POINT ( 'NONE',  ( -7.669357409124427427, -3.748921511560000752, -437.4148671000394302 ) ) ;
#9942 = CARTESIAN_POINT ( 'NONE',  ( 2.737043330023148258, 9.374968016864249520, 315.0000000000000568 ) ) ;
#9943 = DIRECTION ( 'NONE',  ( 0.9554399839384177806, 0.000000000000000000, 0.2951854283188049544 ) ) ;
#9944 = EDGE_LOOP ( 'NONE', ( #6370, #6525, #7727, #2034, #5241, #3529, #5094 ) ) ;
#9945 = EDGE_CURVE ( 'NONE', #7113, #8191, #5741, .T. ) ;
#9946 = CIRCLE ( 'NONE', #855, 13.00000000000001599 ) ;
#9947 = CARTESIAN_POINT ( 'NONE',  ( -1.803054005006139882, -2.571757231099727647, -434.7497522307571103 ) ) ;
#9948 = AXIS2_PLACEMENT_3D ( 'NONE', #3636, #1209, #4440 ) ;
#9949 =( NAMED_UNIT ( * ) SI_UNIT ( $, .STERADIAN. ) SOLID_ANGLE_UNIT ( ) );
#9950 = CARTESIAN_POINT ( 'NONE',  ( -2.852011294728740154, -7.441500538535999354, -435.0252681240257857 ) ) ;
#9951 = CARTESIAN_POINT ( 'NONE',  ( -16.39029893813008343, 2.501810464458257943, -315.0000000000000568 ) ) ;
#9952 = DIRECTION ( 'NONE',  ( 0.000000000000000000, 1.000000000000000000, -0.000000000000000000 ) ) ;
#9953 = DIRECTION ( 'NONE',  ( 0.000000000000000000, -1.000000000000000000, 0.000000000000000000 ) ) ;
#9954 = CARTESIAN_POINT ( 'NONE',  ( -19.31691132429000390, 3.346581979927999217, -316.3802825947000201 ) ) ;
#9955 = AXIS2_PLACEMENT_3D ( 'NONE', #8049, #3219, #1555 ) ;
#9956 = CARTESIAN_POINT ( 'NONE',  ( 18.20355969383999906, -3.293069710501999925, 320.0000000000000000 ) ) ;
#9957 = EDGE_CURVE ( 'NONE', #1052, #1738, #10277, .T. ) ;
#9958 = CARTESIAN_POINT ( 'NONE',  ( 8.327676564211852650, -5.747092138782196713, -525.7147768702978965 ) ) ;
#9959 = CARTESIAN_POINT ( 'NONE',  ( -19.68871134463705985, -8.000000000000000000, -416.4361005590961327 ) ) ;
#9960 = CARTESIAN_POINT ( 'NONE',  ( 8.021995458420214220, -8.375882622524637000, -315.0000000000000000 ) ) ;
#9961 = EDGE_CURVE ( 'NONE', #4332, #2247, #4322, .T. ) ;
#9962 = ORIENTED_EDGE ( 'NONE', *, *, #4566, .T. ) ;
#9963 = CARTESIAN_POINT ( 'NONE',  ( -17.50000000000126832, 0.7437989020612977287, -315.0000000000001705 ) ) ;
#9964 = ORIENTED_EDGE ( 'NONE', *, *, #7521, .F. ) ;
#9965 = DIRECTION ( 'NONE',  ( 0.000000000000000000, 1.000000000000000000, 0.000000000000000000 ) ) ;
#9966 = ORIENTED_EDGE ( 'NONE', *, *, #10481, .T. ) ;
#9967 = CARTESIAN_POINT ( 'NONE',  ( 13.93620031452002728, -8.972937827676991773, -303.6197174156509391 ) ) ;
#9968 = CARTESIAN_POINT ( 'NONE',  ( -14.29183324405000732, -7.414293696095001884, -317.4928077629770087 ) ) ;
#9969 = ADVANCED_FACE ( 'NONE', ( #5320 ), #2914, .F. ) ;
#9970 = DIRECTION ( 'NONE',  ( -0.9612616959383299964, 0.000000000000000000, -0.2756373558169601945 ) ) ;
#9971 = DIRECTION ( 'NONE',  ( 0.000000000000000000, 0.000000000000000000, 1.000000000000000000 ) ) ;
#9972 = CARTESIAN_POINT ( 'NONE',  ( -18.63306024686997375, 4.746768565380000027, -302.9207377450070453 ) ) ;
#9973 = CARTESIAN_POINT ( 'NONE',  ( 2.381287022736665303E-07, -10.00000000000000000, 315.0000000000000000 ) ) ;
#9974 = ORIENTED_EDGE ( 'NONE', *, *, #2368, .T. ) ;
#9975 = CARTESIAN_POINT ( 'NONE',  ( -0.5535498271043974849, -7.499999952522999891, -434.2938920418101816 ) ) ;
#9976 = CARTESIAN_POINT ( 'NONE',  ( -18.32597195921000122, 3.115684853309999891, -302.5000000000129603 ) ) ;
#9977 = ORIENTED_EDGE ( 'NONE', *, *, #6640, .F. ) ;
#9978 = CARTESIAN_POINT ( 'NONE',  ( -19.56039901294001737, 0.5262506252543003304, 189.9229057364800042 ) ) ;
#9979 = CARTESIAN_POINT ( 'NONE',  ( 12.98706127646999953, -6.788989183774999603, -314.4944826805095772 ) ) ;
#9980 = CYLINDRICAL_SURFACE ( 'NONE', #5989, 0.5000000000000128786 ) ;
#9981 = CARTESIAN_POINT ( 'NONE',  ( -77.67426137820133647, -2.500000000000000000, -345.8174414091573681 ) ) ;
#9982 = CARTESIAN_POINT ( 'NONE',  ( -4.854896540501004054, 12.13415599451999682, 191.1197171614399792 ) ) ;
#9983 = EDGE_CURVE ( 'NONE', #9531, #8110, #3136, .T. ) ;
#9984 = CARTESIAN_POINT ( 'NONE',  ( 16.80445917461999983, -3.015803745947999825, 314.4150829855000211 ) ) ;
#9985 = CARTESIAN_POINT ( 'NONE',  ( -72.90663470102438737, -12.50000000000000000, -371.7168990826883714 ) ) ;
#9986 = CARTESIAN_POINT ( 'NONE',  ( -16.74680747859001784, -6.256295688539003308, 320.0770942683900557 ) ) ;
#9987 = AXIS2_PLACEMENT_3D ( 'NONE', #6269, #369, #527 ) ;
#9988 = CARTESIAN_POINT ( 'NONE',  ( -8.203579748838807362, 8.842447418481361510, 314.4999432750971096 ) ) ;
#9989 = CARTESIAN_POINT ( 'NONE',  ( -10.52063983335276554, 10.64371280159997823, -303.5000000000000000 ) ) ;
#9990 = CARTESIAN_POINT ( 'NONE',  ( 10.41198510038999991, 7.677033091942000453, 314.8616023057000461 ) ) ;
#9991 = ORIENTED_EDGE ( 'NONE', *, *, #9047, .T. ) ;
#9992 = CARTESIAN_POINT ( 'NONE',  ( -17.18550143358999449, 2.500000000000000000, -495.8459145668000474 ) ) ;
#9993 = CARTESIAN_POINT ( 'NONE',  ( 19.50549492440999089, 2.789745814424999359, 318.8802828394900644 ) ) ;
#9994 = ORIENTED_EDGE ( 'NONE', *, *, #2679, .T. ) ;
#9995 = VECTOR ( 'NONE', #5979, 1000.000000000000000 ) ;
#9996 = CARTESIAN_POINT ( 'NONE',  ( -4.264364113041657411, -2.626784553234001063, -435.4922059969647421 ) ) ;
#9997 = CARTESIAN_POINT ( 'NONE',  ( 8.900624420096743705, 8.081841135676405941, 314.9999999999999432 ) ) ;
#9999 = EDGE_CURVE ( 'NONE', #1416, #6686, #8396, .T. ) ;
#9998 = CONTEXT_DEPENDENT_SHAPE_REPRESENTATION ( #5781, #6389 ) ;
#10000 = CARTESIAN_POINT ( 'NONE',  ( -2.000000000000000000, 2.500000000000000000, -413.0000000000000000 ) ) ;
#10001 = VERTEX_POINT ( 'NONE', #287 ) ;
#10002 = CARTESIAN_POINT ( 'NONE',  ( -0.7845517089437358260, -2.508978674445781820, -434.2902902441725814 ) ) ;
#10003 = SURFACE_STYLE_FILL_AREA ( #9258 ) ;
#10004 = DIRECTION ( 'NONE',  ( 0.4712473909295827323, 0.000000000000000000, -0.8820010751365675583 ) ) ;
#10005 = DIRECTION ( 'NONE',  ( 0.7220286942758216142, 0.000000000000000000, 0.6918631112021741414 ) ) ;
#10006 = VECTOR ( 'NONE', #1385, 1000.000000000000000 ) ;
#10007 = CARTESIAN_POINT ( 'NONE',  ( -0.2521427309798530136, -2.389480942926001106, -434.5434516125882851 ) ) ;
#10008 = FACE_OUTER_BOUND ( 'NONE', #8289, .T. ) ;
#10009 = DIRECTION ( 'NONE',  ( 0.000000000000000000, -1.000000000000000000, 0.000000000000000000 ) ) ;
#10010 = CARTESIAN_POINT ( 'NONE',  ( -18.02719435607597021, -8.000000000000000000, -431.8467903975401896 ) ) ;
#10011 = CARTESIAN_POINT ( 'NONE',  ( 9.178407731729972596, -5.867721822115068875, -525.3673751052774605 ) ) ;
#10012 = PRODUCT_DEFINITION_CONTEXT ( 'detailed design', #10183, 'design' ) ;
#10013 = CARTESIAN_POINT ( 'NONE',  ( -14.74684780783305449, -5.500000000000000000, -439.3959507452315165 ) ) ;
#10014 = CARTESIAN_POINT ( 'NONE',  ( 13.12058949809353514, -6.031889286829740904, -315.0000000000000000 ) ) ;
#10015 = EDGE_LOOP ( 'NONE', ( #7089, #7334, #9515, #854 ) ) ;
#10016 = CARTESIAN_POINT ( 'NONE',  ( 15.84610571802257795, -4.157530358492036449, -314.5664817403809934 ) ) ;
#10017 = CARTESIAN_POINT ( 'NONE',  ( 19.32351226214660045, -3.349534253028545905, -316.5000000000004547 ) ) ;
#10018 = VERTEX_POINT ( 'NONE', #6900 ) ;
#10019 = CARTESIAN_POINT ( 'NONE',  ( -1.873948611771682149, -12.00000000000000000, -349.2478646809681777 ) ) ;
#10020 = ORIENTED_EDGE ( 'NONE', *, *, #4947, .F. ) ;
#10021 = CARTESIAN_POINT ( 'NONE',  ( 16.93986923087000562, -6.779672025222003739, -302.9207377450070453 ) ) ;
#10022 = ADVANCED_FACE ( 'NONE', ( #9468 ), #8065, .T. ) ;
#10023 = CARTESIAN_POINT ( 'NONE',  ( -15.21494798568001627, -6.716444321683999519, -317.4928077629770087 ) ) ;
#10024 = CARTESIAN_POINT ( 'NONE',  ( -16.92217352393999974, 0.01966449385449000123, -315.0848619657999734 ) ) ;
#10025 = CARTESIAN_POINT ( 'NONE',  ( -16.01368207331000093, 7.610776120867003947, -302.9207377450070453 ) ) ;
#10026 = CARTESIAN_POINT ( 'NONE',  ( -17.50000003227012613, 5.857864393370423528, 314.4997059534069308 ) ) ;
#10027 = ORIENTED_EDGE ( 'NONE', *, *, #8494, .T. ) ;
#10028 = CARTESIAN_POINT ( 'NONE',  ( -0.8407996126558667793, -12.50000000000000000, -352.5919046247526580 ) ) ;
#10029 = EDGE_CURVE ( 'NONE', #5188, #8834, #7827, .T. ) ;
#10030 = CARTESIAN_POINT ( 'NONE',  ( -16.99996037728000076, 1.352916227065999958E-09, 314.9999801883000146 ) ) ;
#10031 = ORIENTED_EDGE ( 'NONE', *, *, #3927, .T. ) ;
#10032 = CARTESIAN_POINT ( 'NONE',  ( 19.98387668437998954, 0.4031290841193003183, 191.1197171614399792 ) ) ;
#10033 = CYLINDRICAL_SURFACE ( 'NONE', #8130, 12.49999999999998757 ) ;
#10034 = CARTESIAN_POINT ( 'NONE',  ( 15.42284054825286432, 3.971008657351323468, -314.9999999999999432 ) ) ;
#10035 = EDGE_CURVE ( 'NONE', #6305, #574, #9169, .T. ) ;
#10036 = CARTESIAN_POINT ( 'NONE',  ( 6.124940582141004342, 11.99257230354999315, 190.4207385301700128 ) ) ;
#10037 = CIRCLE ( 'NONE', #5058, 15.50000000000001421 ) ;
#10038 = VECTOR ( 'NONE', #5244, 1000.000000000000000 ) ;
#10039 = CARTESIAN_POINT ( 'NONE',  ( 17.43193685618000188, -1.405086463480999859, 314.4150829855000211 ) ) ;
#10040 =( LENGTH_UNIT ( ) NAMED_UNIT ( * ) SI_UNIT ( .MILLI., .METRE. ) );
#10041 = DIRECTION ( 'NONE',  ( -0.8820010751365675583, 0.000000000000000000, -0.4712473909295827323 ) ) ;
#10042 = CARTESIAN_POINT ( 'NONE',  ( 17.29814430729002339, -5.659421966102000212, 320.0770942683900557 ) ) ;
#10043 = LINE ( 'NONE', #5954, #2490 ) ;
#10044 = FACE_OUTER_BOUND ( 'NONE', #3356, .T. ) ;
#10045 = CARTESIAN_POINT ( 'NONE',  ( 15.23514566747999943, 4.427644513407000382, 314.8616023057000461 ) ) ;
#10046 = VERTEX_POINT ( 'NONE', #3157 ) ;
#10047 = CARTESIAN_POINT ( 'NONE',  ( 18.68747751655416423, -4.479206664350978251, 190.9999999999995737 ) ) ;
#10048 =( GEOMETRIC_REPRESENTATION_CONTEXT ( 3 ) GLOBAL_UNCERTAINTY_ASSIGNED_CONTEXT ( ( #8186 ) ) GLOBAL_UNIT_ASSIGNED_CONTEXT ( ( #3680, #8224, #7425 ) ) REPRESENTATION_CONTEXT ( 'NONE', 'WORKASPACE' ) );
#10049 = CARTESIAN_POINT ( 'NONE',  ( 10.21681110195000031, 10.83745499882999574, 319.5792614743400009 ) ) ;
#10050 = EDGE_CURVE ( 'NONE', #6593, #24, #1975, .T. ) ;
#10051 = CARTESIAN_POINT ( 'NONE',  ( -12.82747756644705284, -4.303278812719999458, -438.3419432558599738 ) ) ;
#10052 = CARTESIAN_POINT ( 'NONE',  ( -8.586872910504615319, 8.187582572610192955, 315.0000000000000568 ) ) ;
#10053 = CARTESIAN_POINT ( 'NONE',  ( -14.79012398733999945, -1.483731117707000058, -285.0000000000000000 ) ) ;
#10054 = EDGE_LOOP ( 'NONE', ( #1663, #10462 ) ) ;
#10055 = MECHANICAL_DESIGN_GEOMETRIC_PRESENTATION_REPRESENTATION (  '', ( #1127 ), #4050 ) ;
#10056 = CARTESIAN_POINT ( 'NONE',  ( 1.646600138488000020, -11.47371312023999934, -302.5000000000000000 ) ) ;
#10057 = CARTESIAN_POINT ( 'NONE',  ( 10.54676984209158519, -2.500000000000000000, -347.8422498368975084 ) ) ;
#10058 = CARTESIAN_POINT ( 'NONE',  ( 17.35547125580999861, 4.661453509011000307, 190.0000000000000000 ) ) ;
#10059 = CARTESIAN_POINT ( 'NONE',  ( -15.45543459605808145, 3.931565522428363213, -315.0000000000000568 ) ) ;
#10060 = LINE ( 'NONE', #1380, #5472 ) ;
#10061 = CARTESIAN_POINT ( 'NONE',  ( 16.79769345205001585, 5.168336178625003718, 190.0071920248299477 ) ) ;
#10062 = CARTESIAN_POINT ( 'NONE',  ( -72.90663470102438737, -2.599999999999984102, -371.7168990826883714 ) ) ;
#10063 = CARTESIAN_POINT ( 'NONE',  ( -2.000000000000000000, 4.200000000000000178, -409.5000000000000000 ) ) ;
#10064 = CARTESIAN_POINT ( 'NONE',  ( 18.78787853991000034, -1.761062637770999917, 320.0000000000000000 ) ) ;
#10065 = FACE_OUTER_BOUND ( 'NONE', #6578, .T. ) ;
#10066 = CARTESIAN_POINT ( 'NONE',  ( -33.34106825788445150, -7.500000000000000000, -439.6766126514281154 ) ) ;
#10067 = ORIENTED_EDGE ( 'NONE', *, *, #2610, .T. ) ;
#10068 = CARTESIAN_POINT ( 'NONE',  ( 14.00000000000000000, -2.500000000000000000, -317.5000000000000000 ) ) ;
#10069 = DIRECTION ( 'NONE',  ( -0.6276613564377037102, 0.000000000000000000, 0.7784864941890654588 ) ) ;
#10070 = ORIENTED_EDGE ( 'NONE', *, *, #8880, .F. ) ;
#10071 = FACE_OUTER_BOUND ( 'NONE', #5829, .T. ) ;
#10072 = ORIENTED_EDGE ( 'NONE', *, *, #2264, .F. ) ;
#10073 = DIRECTION ( 'NONE',  ( 0.000000000000000000, -1.000000000000000000, 0.000000000000000000 ) ) ;
#10074 = EDGE_CURVE ( 'NONE', #8561, #5927, #4072, .T. ) ;
#10075 = CARTESIAN_POINT ( 'NONE',  ( 19.56018822079001040, 0.5268747006259002497, -317.5770954168139610 ) ) ;
#10076 = CARTESIAN_POINT ( 'NONE',  ( -16.10362618234000109, 3.713712614977999760, -314.6383426456000052 ) ) ;
#10077 = CARTESIAN_POINT ( 'NONE',  ( -19.98289592923002544, -0.4160572288964003440, -303.6197174156509391 ) ) ;
#10078 = DIRECTION ( 'NONE',  ( 0.000000000000000000, 1.000000000000000000, -0.000000000000000000 ) ) ;
#10079 = ORIENTED_EDGE ( 'NONE', *, *, #3389, .T. ) ;
#10080 = CARTESIAN_POINT ( 'NONE',  ( 18.53285823922000120, -2.549737172213000225, 190.0000000000000000 ) ) ;
#10081 = EDGE_CURVE ( 'NONE', #5909, #514, #10525, .T. ) ;
#10082 = DIRECTION ( 'NONE',  ( -1.851488540501311038E-13, -1.000000000000000000, -2.280691893048128447E-14 ) ) ;
#10083 = EDGE_LOOP ( 'NONE', ( #5659, #7982, #3839, #4248 ) ) ;
#10084 = CARTESIAN_POINT ( 'NONE',  ( 10.15702342499999844, -10.85948264422000165, 190.4207385301700128 ) ) ;
#10085 = CARTESIAN_POINT ( 'NONE',  ( -71.87348570190857799, -12.50000000000000000, -375.0609390264727949 ) ) ;
#10086 = CARTESIAN_POINT ( 'NONE',  ( 18.29625743176001862, -2.888693746018001107, -302.5071922382879279 ) ) ;
#10087 = CARTESIAN_POINT ( 'NONE',  ( 2.655864369898997435, 12.48600887025999029, 190.4207385301700128 ) ) ;
#10088 = VECTOR ( 'NONE', #2332, 1000.000000000000000 ) ;
#10089 = CARTESIAN_POINT ( 'NONE',  ( -1.457510205898610467, -7.472866546578002200, -434.5559982538129589 ) ) ;
#10090 = EDGE_CURVE ( 'NONE', #1085, #10392, #10265, .T. ) ;
#10091 = CARTESIAN_POINT ( 'NONE',  ( -78.09771732525952359, -7.656480000000000175, -330.1706946207383453 ) ) ;
#10092 = CARTESIAN_POINT ( 'NONE',  ( 0.6354225718825003977, -12.59144946217000260, 319.5792614743400009 ) ) ;
#10093 = AXIS2_PLACEMENT_3D ( 'NONE', #8686, #9503, #4502 ) ;
#10094 = CARTESIAN_POINT ( 'NONE',  ( -15.42213741511416458, 4.758712124319814940, 314.4999411224990240 ) ) ;
#10095 = CARTESIAN_POINT ( 'NONE',  ( 17.12432750374000179, 0.4000877216259000058, -314.8616023057000461 ) ) ;
#10096 = CARTESIAN_POINT ( 'NONE',  ( 16.54291557298000370, 1.991497705781999805, 315.0848619657999734 ) ) ;
#10097 = EDGE_LOOP ( 'NONE', ( #5964, #6043, #3937, #837 ) ) ;
#10098 = CARTESIAN_POINT ( 'NONE',  ( -6.109815047729933113, -11.91693857169684989, 190.9999999999995737 ) ) ;
#10099 = CARTESIAN_POINT ( 'NONE',  ( 18.77791317464001608, 4.479224074632002228, 319.5792614743400009 ) ) ;
#10100 = CARTESIAN_POINT ( 'NONE',  ( -12.01465775597979935, -3.056837257450998102, -437.6905913349352204 ) ) ;
#10101 = CARTESIAN_POINT ( 'NONE',  ( -4.603463306792016319, 9.141632142122212201, 315.0000000000000568 ) ) ;
#10102 = DIRECTION ( 'NONE',  ( -0.8817975988108817109, 2.326394606397485120E-15, -0.4716280258120411073 ) ) ;
#10103 =( REPRESENTATION_RELATIONSHIP ('NONE','NONE', #8468, #1806 ) REPRESENTATION_RELATIONSHIP_WITH_TRANSFORMATION ( #7418 )SHAPE_REPRESENTATION_RELATIONSHIP( ) );
#10104 = CARTESIAN_POINT ( 'NONE',  ( -7.774319915545000015, -10.49237824600999858, -302.5000000000000000 ) ) ;
#10105 = LINE ( 'NONE', #2747, #2309 ) ;
#10106 = CARTESIAN_POINT ( 'NONE',  ( 16.27511603407000251, 5.909078865696000271, 190.0000000000000000 ) ) ;
#10107 = CARTESIAN_POINT ( 'NONE',  ( 3.206477836452071184, -9.870911208880196241, 314.4999441614608031 ) ) ;
#10108 = CARTESIAN_POINT ( 'NONE',  ( 12.48652197162000554, 8.514177154860004038, 190.0071920248299477 ) ) ;
#10109 = DIRECTION ( 'NONE',  ( 0.000000000000000000, -1.000000000000000000, 0.000000000000000000 ) ) ;
#10110 = CARTESIAN_POINT ( 'NONE',  ( 8.413421927184343119, -4.241283675082794247, -525.6983829592555821 ) ) ;
#10111 = VECTOR ( 'NONE', #8629, 999.9999999999998863 ) ;
#10112 = AXIS2_PLACEMENT_3D ( 'NONE', #7667, #1919, #2932 ) ;
#10113 = CARTESIAN_POINT ( 'NONE',  ( 8.333641625544045084, -5.747896767544797392, -525.7137649939094217 ) ) ;
#10114 = DIRECTION ( 'NONE',  ( 0.000000000000000000, 0.000000000000000000, 1.000000000000000000 ) ) ;
#10115 = ORIENTED_EDGE ( 'NONE', *, *, #342, .T. ) ;
#10116 = CARTESIAN_POINT ( 'NONE',  ( 17.75416867407000154, 3.856294574926997232, 319.9928079742500131 ) ) ;
#10117 = LINE ( 'NONE', #2758, #926 ) ;
#10118 = ORIENTED_EDGE ( 'NONE', *, *, #7206, .T. ) ;
#10119 = LINE ( 'NONE', #7800, #44 ) ;
#10120 = ORIENTED_EDGE ( 'NONE', *, *, #6931, .F. ) ;
#10121 = CARTESIAN_POINT ( 'NONE',  ( -3.630810623869999976, 11.17897874952999793, -317.4928077629770087 ) ) ;
#10122 = CIRCLE ( 'NONE', #6868, 1.000000000000021982 ) ;
#10123 = CARTESIAN_POINT ( 'NONE',  ( -19.46050885281001896, -1.651188223417001444, -317.5770954168139610 ) ) ;
#10124 = CARTESIAN_POINT ( 'NONE',  ( -15.27200851150000105, 4.387263554753999983, -314.8616023057000461 ) ) ;
#10125 = AXIS2_PLACEMENT_3D ( 'NONE', #3337, #9943, #2586 ) ;
#10126 = CARTESIAN_POINT ( 'NONE',  ( -0.8407996126558667793, -12.50000000000000000, -352.5919046247526580 ) ) ;
#10127 = CARTESIAN_POINT ( 'NONE',  ( -38.59226537204000351, -2.500000000000000000, -500.7880554352000217 ) ) ;
#10128 = ORIENTED_EDGE ( 'NONE', *, *, #114, .F. ) ;
#10129 = CARTESIAN_POINT ( 'NONE',  ( -15.64479012893000132, -6.500532800106000764, 190.0000000000000000 ) ) ;
#10130 = CARTESIAN_POINT ( 'NONE',  ( -45.24937426871918689, -2.500000000000000000, -448.9804009737068213 ) ) ;
#10131 = VERTEX_POINT ( 'NONE', #8959 ) ;
#10132 = CARTESIAN_POINT ( 'NONE',  ( -19.86884641856056888, 1.746738893747494803, -316.5000000000005116 ) ) ;
#10133 = ORIENTED_EDGE ( 'NONE', *, *, #8242, .T. ) ;
#10134 = LINE ( 'NONE', #5445, #9669 ) ;
#10135 = CARTESIAN_POINT ( 'NONE',  ( -43.46674421124934184, -9.500000000000001776, -402.7790142173016648 ) ) ;
#10136 = CARTESIAN_POINT ( 'NONE',  ( -12.15874467096999645, 9.926591843472005294, 191.1197171614399792 ) ) ;
#10137 = AXIS2_PLACEMENT_3D ( 'NONE', #8226, #9952, #8179 ) ;
#10138 = MECHANICAL_DESIGN_GEOMETRIC_PRESENTATION_REPRESENTATION (  '', ( #4138 ), #9290 ) ;
#10139 = CARTESIAN_POINT ( 'NONE',  ( -85.25464975288055314, -2.500000000000000000, -378.3143625557585779 ) ) ;
#10140 = DIRECTION ( 'NONE',  ( 0.000000000000000000, -1.000000000000000000, 0.000000000000000000 ) ) ;
#10141 = CARTESIAN_POINT ( 'NONE',  ( -20.05691220054001178, 0.5621708077868997622, 319.5792614743400009 ) ) ;
#10142 = DIRECTION ( 'NONE',  ( 0.000000000000000000, -1.000000000000000000, 0.000000000000000000 ) ) ;
#10143 = CARTESIAN_POINT ( 'NONE',  ( -13.24479143485999977, 5.858166912337999577, 315.0848619657999734 ) ) ;
#10144 = ORIENTED_EDGE ( 'NONE', *, *, #3063, .F. ) ;
#10145 = CARTESIAN_POINT ( 'NONE',  ( -16.34828874915077179, -7.214440038016814327, 190.9999999999995737 ) ) ;
#10146 = ORIENTED_EDGE ( 'NONE', *, *, #6263, .T. ) ;
#10147 = CARTESIAN_POINT ( 'NONE',  ( 9.073652982438993320, 11.14186456285000126, 318.8802828394900644 ) ) ;
#10148 = VECTOR ( 'NONE', #916, 1000.000000000000000 ) ;
#10149 = EDGE_CURVE ( 'NONE', #10381, #4813, #1605, .T. ) ;
#10150 = EDGE_CURVE ( 'NONE', #5927, #1373, #2460, .T. ) ;
#10151 = DIRECTION ( 'NONE',  ( 0.9968876850330226080, 0.000000000000000000, -0.07883491250392217486 ) ) ;
#10152 = CARTESIAN_POINT ( 'NONE',  ( -0.3943348293965602824, 9.499921225251823031, 315.0000000000000000 ) ) ;
#10153 = CARTESIAN_POINT ( 'NONE',  ( -11.71572875295034066, -12.49999999989693755, 319.0000000000000568 ) ) ;
#10154 =( NAMED_UNIT ( * ) SI_UNIT ( $, .STERADIAN. ) SOLID_ANGLE_UNIT ( ) );
#10155 = CARTESIAN_POINT ( 'NONE',  ( -2.240424119748007481, -7.737646341025000041, -436.4485772352342678 ) ) ;
#10156 = ADVANCED_FACE ( 'NONE', ( #5994 ), #8307, .T. ) ;
#10157 = CARTESIAN_POINT ( 'NONE',  ( 15.42213744428624267, -4.758712092923055970, 314.4999411224989103 ) ) ;
#10159 = CARTESIAN_POINT ( 'NONE',  ( -9.745026809365992193, 9.735374599634990744, 190.0071920248299477 ) ) ;
#10158 = CIRCLE ( 'NONE', #9467, 10.00000000000000533 ) ;
#10160 = DIRECTION ( 'NONE',  ( -0.000000000000000000, 1.000000000000000000, 0.000000000000000000 ) ) ;
#10161 = EDGE_CURVE ( 'NONE', #2769, #8773, #1918, .T. ) ;
#10162 = CARTESIAN_POINT ( 'NONE',  ( -50.24071243418999444, 2.500000000000000000, -414.3237589990000629 ) ) ;
#10163 = CARTESIAN_POINT ( 'NONE',  ( -72.90663470102438737, -2.500000000000000444, -368.3168990826883373 ) ) ;
#10164 = CARTESIAN_POINT ( 'NONE',  ( 16.25530297147532721, -2.761162301196854685, 315.0000000000000000 ) ) ;
#10165 = CARTESIAN_POINT ( 'NONE',  ( -14.57772014836000096, 5.380605385836000565, -314.6383426456000052 ) ) ;
#10166 = AXIS2_PLACEMENT_3D ( 'NONE', #3716, #10224, #9415 ) ;
#10167 = ORIENTED_EDGE ( 'NONE', *, *, #1537, .T. ) ;
#10168 = CARTESIAN_POINT ( 'NONE',  ( -7.221770056846003705, 10.51477558267000667, 319.9928079742500131 ) ) ;
#10169 = FACE_OUTER_BOUND ( 'NONE', #5387, .T. ) ;
#10170 = CARTESIAN_POINT ( 'NONE',  ( -7.659536309752155603, -9.500000000000001776, -398.9184288142485570 ) ) ;
#10171 = VERTEX_POINT ( 'NONE', #4338 ) ;
#10172 = DIRECTION ( 'NONE',  ( -0.3064656130346506968, 0.000000000000000000, 0.9518817300627717692 ) ) ;
#10173 = CARTESIAN_POINT ( 'NONE',  ( 13.97631948628000309, -9.047145764649998867, -317.0792622552969533 ) ) ;
#10174 = EDGE_CURVE ( 'NONE', #886, #8632, #5190, .T. ) ;
#10175 = VECTOR ( 'NONE', #902, 1000.000000000000000 ) ;
#10176 = DIRECTION ( 'NONE',  ( 0.000000000000000000, -1.000000000000000000, 0.000000000000000000 ) ) ;
#10177 =( BOUNDED_CURVE ( )  B_SPLINE_CURVE ( 3, ( #10516, #3865, #5409, #6320, #4668, #2360, #1330 ),
 .UNSPECIFIED., .F., .F. ) 
 B_SPLINE_CURVE_WITH_KNOTS ( ( 4, 3, 4 ),
 ( 0.000000000000000000, 0.4966743198807560544, 1.000000000000000000 ),
 .UNSPECIFIED. ) 
 CURVE ( )  GEOMETRIC_REPRESENTATION_ITEM ( )  RATIONAL_B_SPLINE_CURVE ( ( 0.9922741236635395090, 0.8025456745203689568, 0.8051209666325224168, 1.000000000000000000, 0.8025111867385940068, 0.8025111867385940068, 1.000000000000000000 ) ) 
 REPRESENTATION_ITEM ( '' )  );
#10178 = CARTESIAN_POINT ( 'NONE',  ( -13.22841485905253833, -6.750000122098000155, -437.9939945094035920 ) ) ;
#10179 = B_SPLINE_SURFACE_WITH_KNOTS ( 'NONE', 3, 1, ( 
 ( #2640, #5907 ),
 ( #6832, #9356 ),
 ( #5307, #8533 ),
 ( #10260, #2948 ),
 ( #7834, #7781 ),
 ( #2897, #6221 ),
 ( #4408, #6166 ),
 ( #9305, #1991 ),
 ( #1281, #534 ),
 ( #2091, #7096 ),
 ( #1938, #8688 ),
 ( #5358, #6066 ),
 ( #7683, #5259 ) ),
 .UNSPECIFIED., .F., .F., .F.,
 ( 4, 1, 1, 1, 1, 1, 1, 1, 1, 1, 4 ),
 ( 2, 2 ),
 ( 0.01923076923076999858, 0.09935897435896999530, 0.1794871794871999993, 0.2596153846154000133, 0.3397435897436000274, 0.5000000000000000000, 0.6602564102564000281, 0.7403846153845999867, 0.8205128205128000562, 0.9006410256410000148, 0.9807692307692000844 ),
 ( 0.000000000000000000, 1.000000000000000000 ),
 .UNSPECIFIED. ) ;
#10180 = EDGE_LOOP ( 'NONE', ( #930, #2587, #6742, #5185, #9937, #10433 ) ) ;
#10181 = DIRECTION ( 'NONE',  ( 0.000000000000000000, 1.000000000000000000, 0.000000000000000000 ) ) ;
#10182 = CARTESIAN_POINT ( 'NONE',  ( -37.57635160138833896, -9.500000000000001776, -403.2777420460153053 ) ) ;
#10183 = APPLICATION_CONTEXT ( 'automotive_design' ) ;
#10184 = VECTOR ( 'NONE', #6413, 1000.000000000000000 ) ;
#10185 = ORIENTED_EDGE ( 'NONE', *, *, #5677, .F. ) ;
#10186 = CARTESIAN_POINT ( 'NONE',  ( 4.854896540501004054, -12.13415599451999682, 191.1197171614399792 ) ) ;
#10187 = ORIENTED_EDGE ( 'NONE', *, *, #7054, .F. ) ;
#10188 = CYLINDRICAL_SURFACE ( 'NONE', #1782, 15.00000000000001776 ) ;
#10189 = CARTESIAN_POINT ( 'NONE',  ( -13.31171245337000819, -8.049428572247000702, -302.5071922382879279 ) ) ;
#10190 = CIRCLE ( 'NONE', #3845, 14.00000000000000888 ) ;
#10191 = CARTESIAN_POINT ( 'NONE',  ( -79.04021210711869116, -7.500000000000000000, -328.4066924704651456 ) ) ;
#10192 = EDGE_CURVE ( 'NONE', #4191, #8445, #7452, .T. ) ;
#10193 = COLOUR_RGB ( '', 0.31764706, 0.68627451, 0.89019608) ;
#10194 = CARTESIAN_POINT ( 'NONE',  ( -1.073151323001753310, -7.490579005208001462, -434.3854452274036362 ) ) ;
#10195 = FACE_OUTER_BOUND ( 'NONE', #7148, .T. ) ;
#10196 = CARTESIAN_POINT ( 'NONE',  ( 12.99935040274999487, -9.597679858163006728, 319.5792614743400009 ) ) ;
#10197 = CARTESIAN_POINT ( 'NONE',  ( 28.53863984632670636, -2.500000000000000000, -506.8274460463252353 ) ) ;
#10198 = TOROIDAL_SURFACE ( 'NONE', #4196, 12.00000000000000000, 0.5000000000000000000 ) ;
#10199 = CARTESIAN_POINT ( 'NONE',  ( -16.10362618234000109, 3.713712614977999760, 314.6383426456000052 ) ) ;
#10200 = ORIENTED_EDGE ( 'NONE', *, *, #8619, .T. ) ;
#10201 = CIRCLE ( 'NONE', #1963, 19.99999999999999289 ) ;
#10202 = CARTESIAN_POINT ( 'NONE',  ( -18.71194885756699477, -4.439033925638975475, 190.9999999999995737 ) ) ;
#10203 = EDGE_LOOP ( 'NONE', ( #2561, #7080, #3734, #8028 ) ) ;
#10204 = CARTESIAN_POINT ( 'NONE',  ( 7.846787046322997838, 11.50147725199999371, 318.8802828394900644 ) ) ;
#10205 = AXIS2_PLACEMENT_3D ( 'NONE', #8984, #2534, #2589 ) ;
#10206 = AXIS2_PLACEMENT_3D ( 'NONE', #8948, #5770, #9058 ) ;
#10207 = EDGE_CURVE ( 'NONE', #1519, #10171, #5135, .T. ) ;
#10208 = DIRECTION ( 'NONE',  ( 0.000000000000000000, -1.000000000000000000, 0.000000000000000000 ) ) ;
#10209 = CARTESIAN_POINT ( 'NONE',  ( -15.42265167804419512, 3.971230633025111700, 315.0000000000000568 ) ) ;
#10210 = CARTESIAN_POINT ( 'NONE',  ( 19.99999999999999289, -7.322330470418032533, 190.9999999999999432 ) ) ;
#10211 = AXIS2_PLACEMENT_3D ( 'NONE', #10469, #699, #7199 ) ;
#10212 = AXIS2_PLACEMENT_3D ( 'NONE', #1701, #4974, #7448 ) ;
#10213 = CARTESIAN_POINT ( 'NONE',  ( -15.40306756913855679, -3.994766537461137634, -315.0000000000001137 ) ) ;
#10214 = LINE ( 'NONE', #2851, #6078 ) ;
#10215 = ADVANCED_FACE ( 'NONE', ( #2514 ), #1173, .F. ) ;
#10216 = CARTESIAN_POINT ( 'NONE',  ( -46.36553117871467578, -7.500000000000000888, -417.8035921883502510 ) ) ;
#10217 = DIRECTION ( 'NONE',  ( -0.9612616959383172288, 0.000000000000000000, -0.2756373558170051030 ) ) ;
#10218 = EDGE_CURVE ( 'NONE', #10253, #7180, #2121, .T. ) ;
#10219 = CARTESIAN_POINT ( 'NONE',  ( -14.00145308865742422, 5.362717611231083481, -315.0000000000000568 ) ) ;
#10220 = CARTESIAN_POINT ( 'NONE',  ( -18.69235161570000159, 1.652152683404002342, 190.0071920248299477 ) ) ;
#10221 = CYLINDRICAL_SURFACE ( 'NONE', #3028, 19.99999999999999289 ) ;
#10222 = CARTESIAN_POINT ( 'NONE',  ( 14.34749558092999777, -7.521529436904000221, -317.5000000000000000 ) ) ;
#10223 = PRESENTATION_LAYER_ASSIGNMENT (  '', '', ( #784 ) ) ;
#10224 = DIRECTION ( 'NONE',  ( 0.000000000000000000, 0.000000000000000000, -1.000000000000000000 ) ) ;
#10225 = CARTESIAN_POINT ( 'NONE',  ( 13.37739799451331457, -5.841934623551301442, 315.0000000000000000 ) ) ;
#10226 = CARTESIAN_POINT ( 'NONE',  ( -10.40890489166000066, 7.434429060800999522, -315.0848619657999734 ) ) ;
#10227 = EDGE_CURVE ( 'NONE', #4863, #3194, #9927, .T. ) ;
#10228 = EDGE_LOOP ( 'NONE', ( #664, #9861, #840, #4159, #4715, #2656 ) ) ;
#10229 = CARTESIAN_POINT ( 'NONE',  ( -14.87701781886999086, 6.977856518223995330, 319.9928079742500131 ) ) ;
#10230 = CARTESIAN_POINT ( 'NONE',  ( 6.752884998590677590, -11.77766676623698494, -316.5000000000004547 ) ) ;
#10231 = DIRECTION ( 'NONE',  ( 0.000000000000000000, 1.000000000000000000, -0.000000000000000000 ) ) ;
#10232 = ORIENTED_EDGE ( 'NONE', *, *, #10530, .F. ) ;
#10233 = CARTESIAN_POINT ( 'NONE',  ( 10.06352840551000050, 9.619263554820991047, -317.4928077629770087 ) ) ;
#10234 = AXIS2_PLACEMENT_3D ( 'NONE', #8591, #5637, #4792 ) ;
#10235 = CARTESIAN_POINT ( 'NONE',  ( -18.60752753902997725, -4.785892219302998463, -317.0792622552969533 ) ) ;
#10236 = DIRECTION ( 'NONE',  ( 0.09270529807100655328, 0.000000000000000000, -0.9956935912767369556 ) ) ;
#10237 = CARTESIAN_POINT ( 'NONE',  ( 12.32755932899228846, 7.043638358068010419, -314.5741798689287521 ) ) ;
#10238 = ORIENTED_EDGE ( 'NONE', *, *, #8908, .T. ) ;
#10239 = CARTESIAN_POINT ( 'NONE',  ( -7.347903365571999856, -10.60600056872999986, 190.0000000000000000 ) ) ;
#10240 = FACE_BOUND ( 'NONE', #6045, .T. ) ;
#10241 = ORIENTED_EDGE ( 'NONE', *, *, #4033, .F. ) ;
#10242 = CARTESIAN_POINT ( 'NONE',  ( 3.128426543399003279, -12.35671765842998582, 191.1197171614399792 ) ) ;
#10243 = ORIENTED_EDGE ( 'NONE', *, *, #8044, .F. ) ;
#10244 = DIRECTION ( 'NONE',  ( 0.000000000000000000, -1.000000000000000000, 0.000000000000000000 ) ) ;
#10245 = FACE_OUTER_BOUND ( 'NONE', #2458, .T. ) ;
#10246 = ORIENTED_EDGE ( 'NONE', *, *, #7837, .F. ) ;
#10247 =( BOUNDED_SURFACE ( )  B_SPLINE_SURFACE ( 3, 1, ( 
 ( #7734, #3650 ),
 ( #9506, #10210 ),
 ( #3603, #2848 ),
 ( #6117, #2147 ),
 ( #10153, #8483 ),
 ( #9405, #5411 ),
 ( #10361, #3003 ) ),
 .UNSPECIFIED., .F., .F., .F. ) 
 B_SPLINE_SURFACE_WITH_KNOTS ( ( 4, 3, 4 ),
 ( 2, 2 ),
 ( 0.000000000000000000, 0.5000000000000000000, 1.000000000000000000 ),
 ( 0.000000000000000000, 1.000000000000000000 ),
 .UNSPECIFIED. ) 
 GEOMETRIC_REPRESENTATION_ITEM ( )  RATIONAL_B_SPLINE_SURFACE ( (
 ( 1.000000000000000000, 1.000000000000000000),
 ( 0.8047378541210479241, 0.8047378541210479241),
 ( 0.8047378541210479241, 0.8047378541210479241),
 ( 1.000000000000000000, 1.000000000000000000),
 ( 0.8047378541210479241, 0.8047378541210479241),
 ( 0.8047378541210479241, 0.8047378541210479241),
 ( 1.000000000000000000, 1.000000000000000000) ) ) 
 REPRESENTATION_ITEM ( '' )  SURFACE ( )  );
#10248 = CARTESIAN_POINT ( 'NONE',  ( 1.525345003100600394, -2.500000000000000000, -348.4143162901089568 ) ) ;
#10249 = CARTESIAN_POINT ( 'NONE',  ( -18.29625743176001862, 2.888693746018001107, -302.5071922382879279 ) ) ;
#10250 = CARTESIAN_POINT ( 'NONE',  ( 13.92742316895000165, -9.072312068102004190, 319.5792614743400009 ) ) ;
#10251 = CARTESIAN_POINT ( 'NONE',  ( 15.74033075358999945, -3.452242816619000010, -315.0848619657999734 ) ) ;
#10252 = CARTESIAN_POINT ( 'NONE',  ( -17.21448334449999962, 1.351716521078000222, 314.6383426456000052 ) ) ;
#10253 = VERTEX_POINT ( 'NONE', #5831 ) ;
#10254 = CARTESIAN_POINT ( 'NONE',  ( -10.60393767981000757, -9.400660304482000740, 190.0071920248299477 ) ) ;
#10255 = EDGE_LOOP ( 'NONE', ( #8513, #2340, #2084, #946 ) ) ;
#10256 = CARTESIAN_POINT ( 'NONE',  ( -15.00000000000325961, -7.547804830080786473E-15, 315.0000000000001705 ) ) ;
#10257 = CARTESIAN_POINT ( 'NONE',  ( -14.00000000000000000, -2.500000000000000000, -317.5000000000000000 ) ) ;
#10258 = TOROIDAL_SURFACE ( 'NONE', #6299, 15.50000000000000000, 0.5000000000000000000 ) ;
#10259 = CARTESIAN_POINT ( 'NONE',  ( -16.31058353111865955, 2.657800654349994129, 315.0000000000000000 ) ) ;
#10260 = CARTESIAN_POINT ( 'NONE',  ( -13.57573464316000056, -3.225916527208000151, -284.9999999999999432 ) ) ;
#10261 = CARTESIAN_POINT ( 'NONE',  ( -11.74249363970098514, -6.849480045866886080, -315.0000000000000568 ) ) ;
#10262 = CARTESIAN_POINT ( 'NONE',  ( -0.9955007295007036738, -2.573504618523215104, -434.8063702403939033 ) ) ;
#10263 = CARTESIAN_POINT ( 'NONE',  ( -28.01838671672000203, 2.500000000000000000, -497.7560445212000104 ) ) ;
#10264 = DIRECTION ( 'NONE',  ( 0.000000000000000000, 0.000000000000000000, 1.000000000000000000 ) ) ;
#10265 =( BOUNDED_CURVE ( )  B_SPLINE_CURVE ( 3, ( #3099, #4721, #4928, #741, #2298, #10513, #8792, #8042, #2357, #1434, #3046, #6542, #6375, #842, #690, #8205, #7138, #3962, #7189, #6432, #7997, #9715, #5567, #7242, #4827, #8904, #8098, #8155, #9658, #4017, #635, #793, #10406, #3910, #10458, #6316, #10622, #9602, #7299, #8853, #10572, #1495, #3214, #6490, #4773, #9768, #3264, #2406 ),
 .UNSPECIFIED., .F., .F. ) 
 B_SPLINE_CURVE_WITH_KNOTS ( ( 4, 1, 1, 1, 1, 1, 1, 1, 1, 1, 1, 1, 1, 1, 1, 1, 1, 1, 1, 1, 1, 1, 1, 1, 1, 1, 1, 1, 1, 1, 1, 1, 1, 1, 1, 1, 1, 1, 1, 1, 1, 1, 1, 1, 1, 4 ),
 ( 0.000000000000000000, 0.01773478386796039155, 0.03606240600880905589, 0.05363178075044054693, 0.07078725724691502241, 0.08782600590454303635, 0.1049244321358658166, 0.1219539535917407574, 0.1389477140559595703, 0.1563980977818864582, 0.1746363666666239378, 0.1934786392176560677, 0.2128025958997292744, 0.2327904454208181428, 0.2535195744865268441, 0.2747166135707194701, 0.2963888843556194419, 0.3192629785013852417, 0.3441555232881245430, 0.3718650194528611563, 0.4028399612510202843, 0.4371448801345994006, 0.4747436484650955357, 0.5142463203427463103, 0.5531490499891782431, 0.5894092591003674553, 0.6223615841373307811, 0.6515869223714267910, 0.6772431252474824248, 0.7004011076752997278, 0.7222184512862190875, 0.7437909259358911340, 0.7652154438741728404, 0.7858628007620030997, 0.8056883297028466506, 0.8249734464625099184, 0.8436696960199339124, 0.8615821821759899191, 0.8789123401951888237, 0.8960241576542978814, 0.9130500659135323271, 0.9300436868742999463, 0.9471989324631474583, 0.9647777872405101096, 0.9830893744542017476, 1.000000000000000000 ),
 .UNSPECIFIED. ) 
 CURVE ( )  GEOMETRIC_REPRESENTATION_ITEM ( )  RATIONAL_B_SPLINE_CURVE ( ( 1.171573003563729509, 1.171573003563729509, 1.171573003563729509, 1.171573003563729509, 1.171573003563729509, 1.171573003563729509, 1.171573003563729509, 1.171573003563729509, 1.171573003563729509, 1.171573003563729509, 1.171573003563729509, 1.171573003563729509, 1.171573003563729509, 1.171573003563729509, 1.171573003563729509, 1.171573003563729509, 1.171573003563729509, 1.171573003563729509, 1.171573003563729509, 1.171573003563729509, 1.171573003563729509, 1.171573003563729509, 1.171573003563729509, 1.171573003563729509, 1.171573003563729509, 1.171573003563729509, 1.171573003563729509, 1.171573003563729509, 1.171573003563729509, 1.171573003563729509, 1.171573003563729509, 1.171573003563729509, 1.171573003563729509, 1.171573003563729509, 1.171573003563729509, 1.171573003563729509, 1.171573003563729509, 1.171573003563729509, 1.171573003563729509, 1.171573003563729509, 1.171573003563729509, 1.171573003563729509, 1.171573003563729509, 1.171573003563729509, 1.171573003563729509, 1.171573003563729509, 1.171573003563729509, 1.171573003563729731 ) ) 
 REPRESENTATION_ITEM ( '' )  );
#10266 = CARTESIAN_POINT ( 'NONE',  ( -11.84501012641003825, 6.794057347756047527, -315.0000000000000000 ) ) ;
#10267 = CARTESIAN_POINT ( 'NONE',  ( -18.44574565965998758, 2.441956922350000614, 190.0071920248299477 ) ) ;
#10268 = CARTESIAN_POINT ( 'NONE',  ( -28.01838671672000203, -2.500000000000000000, -497.7560445212000104 ) ) ;
#10269 = EDGE_CURVE ( 'NONE', #2579, #6040, #1256, .T. ) ;
#10270 = ORIENTED_EDGE ( 'NONE', *, *, #9880, .F. ) ;
#10271 = DIRECTION ( 'NONE',  ( 0.000000000000000000, -1.000000000000000000, 0.000000000000000000 ) ) ;
#10272 = ADVANCED_FACE ( 'NONE', ( #6761 ), #10033, .T. ) ;
#10273 = DIRECTION ( 'NONE',  ( 0.000000000000000000, -1.000000000000000000, 0.000000000000000000 ) ) ;
#10274 = SHAPE_REPRESENTATION_RELATIONSHIP ( 'NONE' , 'NONE' ,  #4020, #4429 ) ;
#10275 = CARTESIAN_POINT ( 'NONE',  ( 8.647614135908284538, -8.167456227882626152, 315.0000000000000568 ) ) ;
#10276 = CARTESIAN_POINT ( 'NONE',  ( -10.58688533405000065, 7.844683714540999553, -314.6383426456000052 ) ) ;
#10277 = LINE ( 'NONE', #6846, #1630 ) ;
#10278 = CARTESIAN_POINT ( 'NONE',  ( -51.72607275331812104, -12.50000000000000000, -370.6966883942067739 ) ) ;
#10279 = CARTESIAN_POINT ( 'NONE',  ( -5.563766465756743607, -7.500000000000000888, -337.3048648817380126 ) ) ;
#10280 = ORIENTED_EDGE ( 'NONE', *, *, #3332, .F. ) ;
#10281 = CARTESIAN_POINT ( 'NONE',  ( -3.713744197507001576, 11.87335072286999527, -317.5770954168139610 ) ) ;
#10282 = CARTESIAN_POINT ( 'NONE',  ( -12.84330733966000437, -9.683159015349998455, -317.0792622552969533 ) ) ;
#10283 = CARTESIAN_POINT ( 'NONE',  ( -8.037373804805000077, -9.179324345868998591, -315.0000000000000000 ) ) ;
#10284 = EDGE_CURVE ( 'NONE', #3885, #982, #6812, .T. ) ;
#10285 = CARTESIAN_POINT ( 'NONE',  ( -1.822666172895162529, 9.956379168149535275, -314.5031572587578239 ) ) ;
#10286 = ORIENTED_EDGE ( 'NONE', *, *, #1003, .F. ) ;
#10287 = CARTESIAN_POINT ( 'NONE',  ( -11.56195786956000049, -9.110631795823000090, 190.0000000000000000 ) ) ;
#10288 = CIRCLE ( 'NONE', #3604, 0.9999999999999755751 ) ;
#10289 = AXIS2_PLACEMENT_3D ( 'NONE', #9631, #5597, #1521 ) ;
#10290 = CARTESIAN_POINT ( 'NONE',  ( -78.61675616006050404, -7.500000000000000000, -344.0534392588842252 ) ) ;
#10291 = ORIENTED_EDGE ( 'NONE', *, *, #6882, .T. ) ;
#10292 = CARTESIAN_POINT ( 'NONE',  ( -19.50564046359999537, -2.789525877152000621, 191.1197171614399792 ) ) ;
#10293 = ORIENTED_EDGE ( 'NONE', *, *, #4443, .F. ) ;
#10294 = CARTESIAN_POINT ( 'NONE',  ( -16.24439548573774417, -2.790585206482182556, 315.0000000000000000 ) ) ;
#10295 = CARTESIAN_POINT ( 'NONE',  ( 14.33246323392999422, -7.385748264902002092, -302.5071922382879279 ) ) ;
#10296 = EDGE_CURVE ( 'NONE', #8202, #1052, #10134, .T. ) ;
#10297 = CARTESIAN_POINT ( 'NONE',  ( 8.833609186824004311, 11.21733050393000575, 191.1197171614399792 ) ) ;
#10298 = VECTOR ( 'NONE', #4504, 1000.000000000000000 ) ;
#10299 = CARTESIAN_POINT ( 'NONE',  ( -1.941306618757602687, -7.448794727589000075, -434.7455987018001906 ) ) ;
#10300 = CARTESIAN_POINT ( 'NONE',  ( -18.90089112233000179, 0.2930644900430999789, -302.5071922382879279 ) ) ;
#10301 = CARTESIAN_POINT ( 'NONE',  ( -17.10170768143997932, -6.605950023609995725, 319.5792614743400009 ) ) ;
#10302 = CARTESIAN_POINT ( 'NONE',  ( 17.57673583306999632, 0.3313182897943000582, -314.4150829855000211 ) ) ;
#10303 = CARTESIAN_POINT ( 'NONE',  ( -17.56758064089999749, 0.6313722887073999201, 314.4150829855000211 ) ) ;
#10304 = ORIENTED_EDGE ( 'NONE', *, *, #5553, .T. ) ;
#10305 = CARTESIAN_POINT ( 'NONE',  ( 18.12330621507001638, -3.185864752952001222, 190.0071920248299477 ) ) ;
#10306 = CARTESIAN_POINT ( 'NONE',  ( -1.522216677011161368, -7.445310505451432803, -434.6409043759791189 ) ) ;
#10307 = LINE ( 'NONE', #4664, #10111 ) ;
#10308 = ADVANCED_FACE ( 'NONE', ( #5392, #1972, #6149 ), #357, .T. ) ;
#10309 = FACE_BOUND ( 'NONE', #7949, .T. ) ;
#10310 = DIRECTION ( 'NONE',  ( 0.000000000000000000, 1.000000000000000000, 0.000000000000000000 ) ) ;
#10311 = CARTESIAN_POINT ( 'NONE',  ( -14.25090727152774228, 5.161646102170217354, 315.0000000000000568 ) ) ;
#10312 = CARTESIAN_POINT ( 'NONE',  ( -13.89455516181870642, -5.448669939092228631, -314.9999999999999432 ) ) ;
#10313 = CARTESIAN_POINT ( 'NONE',  ( -3.842134514272915524, -2.985559382381202553, -436.1738895293993892 ) ) ;
#10314 = FACE_OUTER_BOUND ( 'NONE', #8786, .T. ) ;
#10315 = CARTESIAN_POINT ( 'NONE',  ( 8.616488358140820480, 8.177789738293624211, -315.0000000000000000 ) ) ;
#10316 = CARTESIAN_POINT ( 'NONE',  ( 18.86321946521001180, -0.4765678057151002123, 190.0071920248299477 ) ) ;
#10317 = CARTESIAN_POINT ( 'NONE',  ( -17.50000000000001776, 8.653894624238266756E-10, -302.5000000000001137 ) ) ;
#10318 = ORIENTED_EDGE ( 'NONE', *, *, #3468, .F. ) ;
#10319 = CARTESIAN_POINT ( 'NONE',  ( 18.32558628770999931, -3.116746082530000184, -317.4999999999870397 ) ) ;
#10320 = DIRECTION ( 'NONE',  ( 1.000000000000000000, 0.000000000000000000, 0.000000000000000000 ) ) ;
#10321 = CARTESIAN_POINT ( 'NONE',  ( 8.586872910504615319, -8.187582572610192955, 315.0000000000000568 ) ) ;
#10322 = CARTESIAN_POINT ( 'NONE',  ( -3.971626792229000280, 9.186906450543000702, -315.0848619657999734 ) ) ;
#10323 = CARTESIAN_POINT ( 'NONE',  ( -12.89405912172824920, -6.798013172113485325, 314.4999472004059839 ) ) ;
#10324 = AXIS2_PLACEMENT_3D ( 'NONE', #9193, #7517, #3435 ) ;
#10325 = CARTESIAN_POINT ( 'NONE',  ( 19.59064078059999758, 0.07061976926606000626, 320.0770942683900557 ) ) ;
#10326 = CARTESIAN_POINT ( 'NONE',  ( -1.582650547086741799, -7.339339277715000165, -435.1382983596024019 ) ) ;
#10327 = CARTESIAN_POINT ( 'NONE',  ( -0.9740888417759976381, -2.575554204550001280, -434.5596432194157615 ) ) ;
#10328 = ORIENTED_EDGE ( 'NONE', *, *, #5932, .T. ) ;
#10329 = CARTESIAN_POINT ( 'NONE',  ( 7.757100520214003758, 11.09835178152000168, -317.5770954168139610 ) ) ;
#10330 = CARTESIAN_POINT ( 'NONE',  ( -10.49155472272000011, -10.73755170802999714, -317.0792622552969533 ) ) ;
#10331 = PRODUCT ( 'Secondary Linkage Connector', 'Secondary Linkage Connector', '', ( #2374 ) ) ;
#10332 = VECTOR ( 'NONE', #2009, 1000.000000000000000 ) ;
#10333 = LINE ( 'NONE', #1250, #4144 ) ;
#10334 = CIRCLE ( 'NONE', #3993, 12.50000000000002309 ) ;
#10335 = CARTESIAN_POINT ( 'NONE',  ( 17.03769437857128821, 2.221013643562902651, -314.5274634404338485 ) ) ;
#10336 = ORIENTED_EDGE ( 'NONE', *, *, #9703, .F. ) ;
#10337 = CARTESIAN_POINT ( 'NONE',  ( -6.244201582844205234, -6.675757048814958239, -437.0437999513653153 ) ) ;
#10338 = EDGE_CURVE ( 'NONE', #10018, #6553, #8811, .T. ) ;
#10339 = CARTESIAN_POINT ( 'NONE',  ( 16.30951479290585482, -7.248637510199255729, 319.0000000000003979 ) ) ;
#10340 = EDGE_LOOP ( 'NONE', ( #3185, #4335, #164, #1271 ) ) ;
#10341 = LINE ( 'NONE', #1364, #9316 ) ;
#10342 = ORIENTED_EDGE ( 'NONE', *, *, #4909, .F. ) ;
#10343 = CARTESIAN_POINT ( 'NONE',  ( -16.45391189178886293, -2.370722300009959760, 315.0000000000001705 ) ) ;
#10344 = CARTESIAN_POINT ( 'NONE',  ( -9.183684135703998663, -10.67340332910999834, -302.4229045757450081 ) ) ;
#10345 = CARTESIAN_POINT ( 'NONE',  ( 14.79481407445002183, 8.414248563823001348, 191.1197171614399792 ) ) ;
#10346 = AXIS2_PLACEMENT_3D ( 'NONE', #7306, #8050, #5736 ) ;
#10347 = ORIENTED_EDGE ( 'NONE', *, *, #2013, .T. ) ;
#10348 = CARTESIAN_POINT ( 'NONE',  ( -0.3480625055678318036, -7.541428400184998715, -433.9440080516719149 ) ) ;
#10349 = SURFACE_STYLE_USAGE ( .BOTH. , #4764 ) ;
#10350 = CARTESIAN_POINT ( 'NONE',  ( -16.10169247195999631, 5.923112460043001626, -302.5071922382879279 ) ) ;
#10351 = DIRECTION ( 'NONE',  ( -3.598068982224053087E-13, -1.000000000000000000, -1.111631867509189775E-13 ) ) ;
#10352 = CARTESIAN_POINT ( 'NONE',  ( 10.67587555525000020, -8.049811041411000900, -314.4150829855000211 ) ) ;
#10353 = CARTESIAN_POINT ( 'NONE',  ( -16.90798586812000082, -0.2930809059028999797, 315.0848619657999734 ) ) ;
#10354 = ORIENTED_EDGE ( 'NONE', *, *, #7939, .F. ) ;
#10355 = DIRECTION ( 'NONE',  ( 0.000000000000000000, -1.000000000000000000, 0.000000000000000000 ) ) ;
#10356 = CARTESIAN_POINT ( 'NONE',  ( -0.9220120792583293978, -7.482292487583758422, -434.3711255064411603 ) ) ;
#10357 = CARTESIAN_POINT ( 'NONE',  ( -28.01838671672410896, -2.500000000000000000, -497.7560445212019999 ) ) ;
#10358 = DIRECTION ( 'NONE',  ( -0.000000000000000000, 1.000000000000000000, 0.000000000000000000 ) ) ;
#10359 = FACE_BOUND ( 'NONE', #8189, .T. ) ;
#10360 = CARTESIAN_POINT ( 'NONE',  ( -16.99965680672947954, 0.4176726732850534751, 314.9999999999998863 ) ) ;
#10361 = CARTESIAN_POINT ( 'NONE',  ( -20.00000000000000000, 3.518725546161979705E-10, 319.0000000000000000 ) ) ;
#10362 = CARTESIAN_POINT ( 'NONE',  ( -16.99910511164433302, -0.8673928700097519595, -315.0000000000000000 ) ) ;
#10363 = FACE_OUTER_BOUND ( 'NONE', #7992, .T. ) ;
#10364 = CARTESIAN_POINT ( 'NONE',  ( 17.50000000000002487, 1.995060298004523415E-08, 314.4999385900306947 ) ) ;
#10365 = AXIS2_PLACEMENT_3D ( 'NONE', #6889, #7736, #7948 ) ;
#10366 = CARTESIAN_POINT ( 'NONE',  ( -48.08064548948741646, -9.000000000000001776, -401.8957833228595860 ) ) ;
#10367 = CARTESIAN_POINT ( 'NONE',  ( -11.80659750965543608, 6.814906413124091955, -314.9999999999999432 ) ) ;
#10368 = CARTESIAN_POINT ( 'NONE',  ( -6.317945743273003956, 11.44290306353000730, 189.9229057364800042 ) ) ;
#10369 = CARTESIAN_POINT ( 'NONE',  ( 3.206494179919505694, 9.870881073625612956, 314.4999451744448606 ) ) ;
#10370 = CARTESIAN_POINT ( 'NONE',  ( -7.617198281494000689, -10.53565010756000042, -317.5000000000000000 ) ) ;
#10371 = CIRCLE ( 'NONE', #5917, 13.99999999999999645 ) ;
#10372 = CIRCLE ( 'NONE', #1111, 11.00000000000000000 ) ;
#10373 = PLANE ( 'NONE',  #5794 ) ;
#10374 = PRODUCT_CONTEXT ( 'NONE', #3795, 'mechanical' ) ;
#10375 = CARTESIAN_POINT ( 'NONE',  ( 15.63365740121746406, -3.715179591933191361, 315.0000000000000568 ) ) ;
#10376 = CARTESIAN_POINT ( 'NONE',  ( 8.450675645183000739, 8.177559542660000957, -315.0848619657999734 ) ) ;
#10377 = CARTESIAN_POINT ( 'NONE',  ( -8.203499201192052226, -8.842483654835438855, 314.4999460608030404 ) ) ;
#10378 = CARTESIAN_POINT ( 'NONE',  ( -19.10207382662997588, 2.686351016941002534, 320.0770942683900557 ) ) ;
#10379 = SURFACE_SIDE_STYLE ('',( #3019 ) ) ;
#10380 = CARTESIAN_POINT ( 'NONE',  ( -0.5644360195601177965, -2.523842503971001960, -434.5698867567434149 ) ) ;
#10381 = VERTEX_POINT ( 'NONE', #4483 ) ;
#10382 = CARTESIAN_POINT ( 'NONE',  ( -19.39427072114999717, 3.381181012882998882, -317.0792622552969533 ) ) ;
#10383 = CARTESIAN_POINT ( 'NONE',  ( -13.88920775975001298, -9.001345760802989204, -316.3802825947000201 ) ) ;
#10384 = DIRECTION ( 'NONE',  ( 0.000000000000000000, 1.000000000000000000, -0.000000000000000000 ) ) ;
#10385 = DIRECTION ( 'NONE',  ( 0.9942380540931649024, 0.000000000000000000, 0.1071946444232959872 ) ) ;
#10386 = EDGE_LOOP ( 'NONE', ( #9220, #3378, #6158, #3386, #3584 ) ) ;
#10387 = MECHANICAL_DESIGN_GEOMETRIC_PRESENTATION_REPRESENTATION (  '', ( #4555 ), #8844 ) ;
#10388 = CARTESIAN_POINT ( 'NONE',  ( -17.44177680037102007, -0.9115828329868908009, -314.5029970719331232 ) ) ;
#10389 = ADVANCED_FACE ( 'NONE', ( #7762 ), #5242, .T. ) ;
#10390 = VERTEX_POINT ( 'NONE', #1208 ) ;
#10391 = CARTESIAN_POINT ( 'NONE',  ( -0.2363647329299939648, 12.51727884664820856, -316.5000000000004547 ) ) ;
#10392 = VERTEX_POINT ( 'NONE', #6257 ) ;
#10393 = CARTESIAN_POINT ( 'NONE',  ( -3.689342025446077589, -9.275861061134104801, 315.0000000000001137 ) ) ;
#10394 = CARTESIAN_POINT ( 'NONE',  ( -15.97017057534000450, -7.646575558462997080, -302.9207377450070453 ) ) ;
#10395 = CARTESIAN_POINT ( 'NONE',  ( 15.59929043073998578, 7.826471063572999931, 191.1197171614399792 ) ) ;
#10396 =( LENGTH_UNIT ( ) NAMED_UNIT ( * ) SI_UNIT ( .MILLI., .METRE. ) );
#10397 = EDGE_CURVE ( 'NONE', #7778, #306, #1093, .T. ) ;
#10398 = CARTESIAN_POINT ( 'NONE',  ( 11.73636226353998779, 10.21860227534999943, -302.9207377450070453 ) ) ;
#10399 = CARTESIAN_POINT ( 'NONE',  ( -10.00000000000000000, -2.500000000000000000, -285.0000000000000000 ) ) ;
#10400 = EDGE_LOOP ( 'NONE', ( #9585, #9924, #6527, #4661 ) ) ;
#10401 = CARTESIAN_POINT ( 'NONE',  ( -10.50000150490000017, -7.882579085736000302, -314.6383426456000052 ) ) ;
#10402 = B_SPLINE_CURVE_WITH_KNOTS ( 'NONE', 3,
 ( #6396, #9786, #6616, #4842, #9674, #5747, #4892, #7261, #4943, #8173, #10531, #3929, #9032, #7209, #5586, #4740, #8870, #6450, #2424, #4, #806, #5692, #2529, #753, #1512, #8218, #4089, #9731, #858, #3279, #4037, #10475, #8810, #1459, #7316, #8011, #654, #5962, #9199, #5205, #325, #9997, #8482, #3602, #9304, #5797, #6778, #7628, #1834, #6666, #1124, #273, #2693, #9254, #1883, #3551, #6831, #2584, #9086, #9942, #3498, #1724, #4407, #5046, #10152, #2638, #6885, #5905, #5155, #5101, #8428, #116, #1070, #4355, #7682, #8380, #1015, #10101, #2743, #4304, #220, #6011, #8272, #3391, #10052, #7574, #5847, #9138, #1937, #4993, #8329, #1776, #909, #4198, #7473, #967, #4252, #7523, #166, #3443, #6721, #586, #2947, #7833, #4454, #4559, #10311, #6933, #4669, #3866, #1280, #6220, #10209, #4611, #9556, #7733, #375, #5257, #6065, #10259, #8532, #424, #3702, #7143, #482, #3750, #2195, #8635, #2847, #5410, #6276, #10360, #2895 ),
 .UNSPECIFIED., .F., .F.,
 ( 4, 1, 1, 1, 1, 1, 2, 2, 1, 1, 1, 1, 1, 2, 2, 1, 1, 1, 1, 1, 2, 2, 1, 1, 1, 1, 1, 2, 2, 1, 1, 1, 1, 1, 1, 2, 2, 1, 1, 1, 1, 1, 2, 2, 1, 1, 2, 2, 2, 1, 1, 2, 2, 1, 1, 1, 1, 2, 2, 1, 1, 1, 1, 1, 1, 2, 2, 1, 1, 1, 1, 1, 2, 2, 1, 1, 1, 1, 1, 2, 2, 1, 1, 1, 1, 1, 2, 2, 1, 1, 1, 1, 2, 2, 1, 1, 1, 2, 2, 4 ),
 ( 0.000000000000000000, 0.06250000000000791034, 0.09375000000001181000, 0.1093750000000137529, 0.1171875000000147105, 0.1210937500000152794, 0.1230468750000155709, 0.1250000000000158484, 0.1562500000000223432, 0.1718750000000255906, 0.1796875000000270617, 0.1835937500000277833, 0.1855468750000281719, 0.1865234375000283107, 0.1875000000000284217, 0.2187500000000311418, 0.2343750000000323908, 0.2421875000000330014, 0.2460937500000334177, 0.2480468750000336398, 0.2490234375000336953, 0.2500000000000337508, 0.2812500000000370259, 0.2968750000000386358, 0.3046875000000394684, 0.3085937500000398570, 0.3105468750000400235, 0.3115234375000401346, 0.3125000000000403011, 0.3437500000000445199, 0.3593750000000465739, 0.3671875000000476286, 0.3710937500000481282, 0.3730468750000484057, 0.3740234375000484612, 0.3745117187500484612, 0.3750000000000484612, 0.4062500000000490163, 0.4218750000000493494, 0.4296875000000495159, 0.4335937500000495715, 0.4355468750000495715, 0.4365234375000495715, 0.4375000000000495715, 0.4531250000000494604, 0.4609375000000494049, 0.4648437500000494049, 0.4687500000000494049, 0.5000000000000491829, 0.5156250000000491829, 0.5234375000000491829, 0.5273437500000490719, 0.5312500000000490719, 0.5468750000000488498, 0.5546875000000488498, 0.5585937500000488498, 0.5605468750000488498, 0.5615234375000488498, 0.5625000000000488498, 0.5937500000000481837, 0.6093750000000478506, 0.6171875000000476286, 0.6210937500000475175, 0.6230468750000474065, 0.6240234375000474065, 0.6245117187500474065, 0.6250000000000472955, 0.6562500000000430767, 0.6718750000000409672, 0.6796875000000398570, 0.6835937500000393019, 0.6855468750000390799, 0.6865234375000389688, 0.6875000000000388578, 0.7187500000000363043, 0.7343750000000350830, 0.7421875000000345279, 0.7460937500000343059, 0.7480468750000340838, 0.7490234375000340838, 0.7500000000000340838, 0.7812500000000317524, 0.7968750000000304201, 0.8046875000000298650, 0.8085937500000295319, 0.8105468750000293099, 0.8115234375000293099, 0.8125000000000293099, 0.8437500000000242029, 0.8593750000000216493, 0.8671875000000203171, 0.8710937500000196509, 0.8730468750000193179, 0.8750000000000189848, 0.9062500000000143219, 0.9218750000000121014, 0.9296875000000109912, 0.9335937500000103251, 0.9375000000000097700, 1.000000000000000000 ),
 .UNSPECIFIED. ) ;
#10403 = CARTESIAN_POINT ( 'NONE',  ( -4.143439832052679961, -2.711403837272623463, -435.5329398554599720 ) ) ;
#10404 = VERTEX_POINT ( 'NONE', #6971 ) ;
#10405 = CARTESIAN_POINT ( 'NONE',  ( -19.38229133873998222, -1.780473529460998128, 189.9229057364800042 ) ) ;
#10406 = CARTESIAN_POINT ( 'NONE',  ( 12.04241988217490622, 9.990194130379512316, 190.9999999999996589 ) ) ;
#10407 = CARTESIAN_POINT ( 'NONE',  ( -15.00000000000325961, -7.547804830080786473E-15, -284.9999999999999432 ) ) ;
#10408 = VERTEX_POINT ( 'NONE', #9388 ) ;
#10409 = CARTESIAN_POINT ( 'NONE',  ( -16.98808798087999961, -1.334629195702000004, 314.8616023057000461 ) ) ;
#10410 = FACE_OUTER_BOUND ( 'NONE', #1359, .T. ) ;
#10411 = LINE ( 'NONE', #2249, #732 ) ;
#10412 = CARTESIAN_POINT ( 'NONE',  ( -8.736690731312993563, -10.08117623986000133, 319.9928079742500131 ) ) ;
#10413 = CARTESIAN_POINT ( 'NONE',  ( -2.737481088004029228, -9.377302004685557080, -315.0000000000000000 ) ) ;
#10414 = SURFACE_STYLE_FILL_AREA ( #9724 ) ;
#10415 = CARTESIAN_POINT ( 'NONE',  ( -2.000000000003786749, -9.500000000000001776, -409.4999999999758415 ) ) ;
#10416 = ORIENTED_EDGE ( 'NONE', *, *, #4735, .F. ) ;
#10417 = CARTESIAN_POINT ( 'NONE',  ( -78.09771732525952359, -2.500000000000000000, -330.1706946207383453 ) ) ;
#10418 = CARTESIAN_POINT ( 'NONE',  ( 4.298300662841374020, 9.188610398197571527, -315.0000000000000568 ) ) ;
#10419 = PRODUCT_DEFINITION_SHAPE ( 'NONE', 'NONE',  #3305 ) ;
#10420 = CARTESIAN_POINT ( 'NONE',  ( -7.675832365144997560, 11.11882312068000189, 189.9229057364800042 ) ) ;
#10421 = CARTESIAN_POINT ( 'NONE',  ( 17.50000000088856567, 5.867334121986925055, -302.4999999999996589 ) ) ;
#10422 = ADVANCED_FACE ( 'NONE', ( #517 ), #10188, .F. ) ;
#10423 = VECTOR ( 'NONE', #7363, 1000.000000000000227 ) ;
#10424 = CARTESIAN_POINT ( 'NONE',  ( 3.131429216827940247E-09, -12.50000000000000000, -316.5000000000000000 ) ) ;
#10425 = CARTESIAN_POINT ( 'NONE',  ( -102.0103468492230547, -2.500000000000000000, -289.6591388711787545 ) ) ;
#10426 = SHAPE_DEFINITION_REPRESENTATION ( #2954, #33 ) ;
#10427 = CARTESIAN_POINT ( 'NONE',  ( -17.71378747801018960, -5.838323448755803113, -303.5000000000006253 ) ) ;
#10428 = CARTESIAN_POINT ( 'NONE',  ( -10.00000000000000000, 2.500000000000000000, -272.5000000000000000 ) ) ;
#10429 = CARTESIAN_POINT ( 'NONE',  ( -3.214697847761800006E-15, 10.00000000000000000, 315.0000000000000000 ) ) ;
#10430 = CARTESIAN_POINT ( 'NONE',  ( 18.77022956583000735, 3.456581952569002247, 320.0770942683900557 ) ) ;
#10431 = CARTESIAN_POINT ( 'NONE',  ( -14.81771799810021584, -5.543961357743112828, -439.1069350289280351 ) ) ;
#10432 = CARTESIAN_POINT ( 'NONE',  ( -0.5143507147629048371, -2.516076635578000875, -434.2178808803126913 ) ) ;
#10433 = ORIENTED_EDGE ( 'NONE', *, *, #6585, .F. ) ;
#10434 = CARTESIAN_POINT ( 'NONE',  ( -5.251781279335003383, 11.64703610505998910, -317.5770954168139610 ) ) ;
#10435 = CARTESIAN_POINT ( 'NONE',  ( -6.467159262072997628, -11.83367582535999141, -316.3802825947000201 ) ) ;
#10436 = EDGE_CURVE ( 'NONE', #9806, #1376, #727, .T. ) ;
#10437 = VERTEX_POINT ( 'NONE', #4439 ) ;
#10438 = CARTESIAN_POINT ( 'NONE',  ( -0.3764627761248945381, -12.50000000000000000, -361.1540620660322816 ) ) ;
#10439 = CARTESIAN_POINT ( 'NONE',  ( -17.04726327197863256, 2.225800558269679819, -314.5277276635413273 ) ) ;
#10440 = ORIENTED_EDGE ( 'NONE', *, *, #2330, .T. ) ;
#10441 = CARTESIAN_POINT ( 'NONE',  ( -15.84843729815538538, -4.154783985720819750, -314.5664249374442534 ) ) ;
#10442 = ORIENTED_EDGE ( 'NONE', *, *, #9636, .F. ) ;
#10443 = CARTESIAN_POINT ( 'NONE',  ( -14.97237716209997416, 8.305886502593784471, -316.5000000000004547 ) ) ;
#10444 = VERTEX_POINT ( 'NONE', #5336 ) ;
#10445 = CARTESIAN_POINT ( 'NONE',  ( -11.28384026436728327, -7.096146896414363248, 315.0000000000000000 ) ) ;
#10446 = CARTESIAN_POINT ( 'NONE',  ( -7.921361508960999664, -11.05315760980000661, -302.4229045757450081 ) ) ;
#10447 = DIRECTION ( 'NONE',  ( -0.9712267471052614676, 0.000000000000000000, -0.2381566831044902022 ) ) ;
#10448 =( NAMED_UNIT ( * ) SI_UNIT ( $, .STERADIAN. ) SOLID_ANGLE_UNIT ( ) );
#10449 = CIRCLE ( 'NONE', #2908, 5.000000000000004441 ) ;
#10450 = VECTOR ( 'NONE', #6838, 1000.000000000000227 ) ;
#10451 = CARTESIAN_POINT ( 'NONE',  ( 14.68756396110000395, 7.991310926523999214, -302.4229045757450081 ) ) ;
#10452 = CARTESIAN_POINT ( 'NONE',  ( 19.49027688392999735, -2.831154404542999714, 318.8802828394900644 ) ) ;
#10453 = ORIENTED_EDGE ( 'NONE', *, *, #4791, .F. ) ;
#10454 = CARTESIAN_POINT ( 'NONE',  ( -3.846123575835999731, -9.203727088275000412, -315.0848619657999734 ) ) ;
#10455 = CARTESIAN_POINT ( 'NONE',  ( 13.34617449956999913, 8.168334506422000985, -302.5000000000000000 ) ) ;
#10456 = VERTEX_POINT ( 'NONE', #3635 ) ;
#10457 = CARTESIAN_POINT ( 'NONE',  ( 15.36042613538998758, -7.487426557894995227, 189.9229057364800042 ) ) ;
#10458 = CARTESIAN_POINT ( 'NONE',  ( 13.93599793909949547, 8.976999749472311052, 190.9999999999996589 ) ) ;
#10459 = CARTESIAN_POINT ( 'NONE',  ( -72.90663470102438737, -12.50000000000000000, -371.7168990826883714 ) ) ;
#10460 = VECTOR ( 'NONE', #7356, 1000.000000000000000 ) ;
#10461 = ORIENTED_EDGE ( 'NONE', *, *, #10623, .F. ) ;
#10462 = ORIENTED_EDGE ( 'NONE', *, *, #880, .T. ) ;
#10463 = CARTESIAN_POINT ( 'NONE',  ( -12.10743226551000085, -7.094093637544000686, 314.6383426456000052 ) ) ;
#10464 = DIRECTION ( 'NONE',  ( -6.627266684903556796E-12, 1.000000000000000000, 1.877906674862047561E-12 ) ) ;
#10465 = CARTESIAN_POINT ( 'NONE',  ( -13.45825946928999706, -7.955479052880997770, 319.9928079742500131 ) ) ;
#10466 =( GEOMETRIC_REPRESENTATION_CONTEXT ( 3 ) GLOBAL_UNCERTAINTY_ASSIGNED_CONTEXT ( ( #7434 ) ) GLOBAL_UNIT_ASSIGNED_CONTEXT ( ( #4796, #2322, #2428 ) ) REPRESENTATION_CONTEXT ( 'NONE', 'WORKASPACE' ) );
#10467 = CARTESIAN_POINT ( 'NONE',  ( -11.98824862436842587, 10.01561519341996487, 319.0000000000005116 ) ) ;
#10468 = DIRECTION ( 'NONE',  ( 0.9850643254521072034, 0.000000000000000000, 0.1721867437452284377 ) ) ;
#10469 = CARTESIAN_POINT ( 'NONE',  ( -2.000000000000000000, 3.500000000000000000, -409.5000000000000000 ) ) ;
#10470 = ORIENTED_EDGE ( 'NONE', *, *, #4895, .F. ) ;
#10471 = DIRECTION ( 'NONE',  ( 0.000000000000000000, -1.000000000000000000, 0.000000000000000000 ) ) ;
#10472 = CARTESIAN_POINT ( 'NONE',  ( 18.76999596014998772, 3.457077136807001683, 189.9229057364800042 ) ) ;
#10473 = CARTESIAN_POINT ( 'NONE',  ( 7.551285798577536568, 9.031218586147737426, 314.4999459341804595 ) ) ;
#10474 = DIRECTION ( 'NONE',  ( 0.000000000000000000, 0.000000000000000000, 1.000000000000000000 ) ) ;
#10475 = CARTESIAN_POINT ( 'NONE',  ( 12.11102551177084941, 6.646503028198875285, 314.9999999999999432 ) ) ;
#10476 = APPLICATION_PROTOCOL_DEFINITION ( 'draft international standard', 'automotive_design', 1998, #2153 ) ;
#10477 = CARTESIAN_POINT ( 'NONE',  ( -14.92864611359687999, -8.336576156742355082, -303.4999999999996589 ) ) ;
#10478 = CARTESIAN_POINT ( 'NONE',  ( 17.56330558013000243, 0.6698376231023999150, -314.4150829855000211 ) ) ;
#10479 = EDGE_CURVE ( 'NONE', #2787, #1717, #69, .T. ) ;
#10480 = DIRECTION ( 'NONE',  ( 0.1247904863035921574, 0.000000000000000000, -0.9921831154218020421 ) ) ;
#10481 = EDGE_CURVE ( 'NONE', #7778, #6664, #7666, .T. ) ;
#10482 = CARTESIAN_POINT ( 'NONE',  ( -0.6255878334489998194, 12.09339422449000168, 320.0770942683900557 ) ) ;
#10483 =( NAMED_UNIT ( * ) PLANE_ANGLE_UNIT ( ) SI_UNIT ( $, .RADIAN. ) );
#10484 = CARTESIAN_POINT ( 'NONE',  ( -1.805690315422955994, -2.544311598584000134, -434.6943802261359338 ) ) ;
#10485 = VERTEX_POINT ( 'NONE', #307 ) ;
#10486 = CARTESIAN_POINT ( 'NONE',  ( 18.90056365643000547, 0.3167749459464000994, -317.4928077629770087 ) ) ;
#10487 = CARTESIAN_POINT ( 'NONE',  ( -19.29920617650999404, -3.385971943253997640, -316.3802825947000201 ) ) ;
#10488 = ORIENTED_EDGE ( 'NONE', *, *, #9836, .F. ) ;
#10489 = CARTESIAN_POINT ( 'NONE',  ( 11.54587391409000041, -9.118162486329000060, 320.0000000000000000 ) ) ;
#10490 = FACE_BOUND ( 'NONE', #8942, .T. ) ;
#10491 = LINE ( 'NONE', #3833, #7601 ) ;
#10492 = VERTEX_POINT ( 'NONE', #1260 ) ;
#10493 = CARTESIAN_POINT ( 'NONE',  ( 12.96318846091384991, -9.529552999724860030, 319.0000000000003979 ) ) ;
#10494 = EDGE_CURVE ( 'NONE', #9531, #9273, #811, .T. ) ;
#10495 = ORIENTED_EDGE ( 'NONE', *, *, #1671, .T. ) ;
#10496 = DIRECTION ( 'NONE',  ( 0.000000000000000000, -1.000000000000000000, 0.000000000000000000 ) ) ;
#10497 = ORIENTED_EDGE ( 'NONE', *, *, #6872, .F. ) ;
#10498 = CARTESIAN_POINT ( 'NONE',  ( -4.252796533868254514, -9.197585063050969012, 315.0000000000000568 ) ) ;
#10499 = CARTESIAN_POINT ( 'NONE',  ( -10.56785312427999735, -10.70734743398999811, -302.9207377450070453 ) ) ;
#10500 = B_SPLINE_CURVE_WITH_KNOTS ( 'NONE', 3,
 ( #1997, #4411, #10107, #2749, #6018, #7687, #1132, #6729, #2592, #175, #9260, #5854, #331, #6891, #10157, #5968, #1025, #1839, #4260, #5107, #228, #7530 ),
 .UNSPECIFIED., .F., .F.,
 ( 4, 2, 2, 2, 2, 2, 2, 2, 2, 2, 4 ),
 ( 0.4999983592357296613, 0.5624985643312634398, 0.5937486668790303845, 0.6249987694267972183, 0.6562488719745640520, 0.6874989745223309967, 0.7499991796178647752, 0.8124993847133985536, 0.8749995898089324431, 0.9374997949044662215, 1.000000000000000000 ),
 .UNSPECIFIED. ) ;
#10501 = CARTESIAN_POINT ( 'NONE',  ( -72.90663470096859555, -7.500000000000000000, -371.7168990827444190 ) ) ;
#10502 = VECTOR ( 'NONE', #10355, 1000.000000000000000 ) ;
#10503 = CARTESIAN_POINT ( 'NONE',  ( 0.000000000000000000, -10.00000000000000000, 315.0000000000000000 ) ) ;
#10504 =( LENGTH_UNIT ( ) NAMED_UNIT ( * ) SI_UNIT ( .MILLI., .METRE. ) );
#10505 = CARTESIAN_POINT ( 'NONE',  ( -9.278531818924999897, 11.16715007748999078, -302.9207377450070453 ) ) ;
#10506 = CARTESIAN_POINT ( 'NONE',  ( 18.17597206675998223, -5.223702392620001689, 318.8802828394900644 ) ) ;
#10507 = ORIENTED_EDGE ( 'NONE', *, *, #4259, .F. ) ;
#10508 = CARTESIAN_POINT ( 'NONE',  ( -3.903842856253999738, -9.647088721075000706, -314.6383426456000052 ) ) ;
#10509 = CARTESIAN_POINT ( 'NONE',  ( -17.50000000000000000, 0.000000000000000000, -302.5000000000000000 ) ) ;
#10510 = VECTOR ( 'NONE', #8318, 1000.000000000000000 ) ;
#10511 = EDGE_LOOP ( 'NONE', ( #5850, #7125, #9909, #1504, #7715, #131, #7663, #7597, #7995, #7437, #9419, #9000 ) ) ;
#10512 = CARTESIAN_POINT ( 'NONE',  ( -18.76999596014998772, -3.457077136807001683, 189.9229057364800042 ) ) ;
#10513 = CARTESIAN_POINT ( 'NONE',  ( -19.12881201168725198, 3.682481340332639519, 190.9999999999996589 ) ) ;
#10514 = DIRECTION ( 'NONE',  ( -0.8820010751365653379, 0.000000000000000000, -0.4712473909295871732 ) ) ;
#10515 = CARTESIAN_POINT ( 'NONE',  ( -15.89383674730000173, -3.622219875512000087, 314.8616023057000461 ) ) ;
#10516 = CARTESIAN_POINT ( 'NONE',  ( 0.000000000000000000, -10.00000000000000178, 315.0000000000000000 ) ) ;
#10517 = FACE_OUTER_BOUND ( 'NONE', #5299, .T. ) ;
#10518 = PLANE ( 'NONE',  #7042 ) ;
#10519 = CARTESIAN_POINT ( 'NONE',  ( -13.88765719697804712, 9.006220412848993107, 319.0000000000005116 ) ) ;
#10520 = CARTESIAN_POINT ( 'NONE',  ( -14.85833869408811125, -4.382513931880057889, -438.9412797724170900 ) ) ;
#10521 = CARTESIAN_POINT ( 'NONE',  ( -13.57573464316000056, 3.225916527208000151, 315.0000000000000000 ) ) ;
#10522 = ORIENTED_EDGE ( 'NONE', *, *, #9040, .T. ) ;
#10523 = LINE ( 'NONE', #2255, #2088 ) ;
#10524 = ADVANCED_FACE ( 'NONE', ( #8046 ), #5516, .T. ) ;
#10525 = CIRCLE ( 'NONE', #5721, 5.000000000000004441 ) ;
#10526 = CARTESIAN_POINT ( 'NONE',  ( 8.712128322568002403, 10.82186910204999997, 189.9229057364800042 ) ) ;
#10527 = CARTESIAN_POINT ( 'NONE',  ( -9.285088343770869557, -9.000000000000001776, -419.6576319987959778 ) ) ;
#10528 = EDGE_LOOP ( 'NONE', ( #4326, #2930, #1263, #8082 ) ) ;
#10529 = DIRECTION ( 'NONE',  ( 0.000000000000000000, -1.000000000000000000, 0.000000000000000000 ) ) ;
#10530 = EDGE_CURVE ( 'NONE', #1489, #6903, #3051, .T. ) ;
#10531 = CARTESIAN_POINT ( 'NONE',  ( 16.24439548573774417, 2.790585206482182556, 315.0000000000000000 ) ) ;
#10532 =( GEOMETRIC_REPRESENTATION_CONTEXT ( 3 ) GLOBAL_UNCERTAINTY_ASSIGNED_CONTEXT ( ( #8077 ) ) GLOBAL_UNIT_ASSIGNED_CONTEXT ( ( #5105, #1941, #9949 ) ) REPRESENTATION_CONTEXT ( 'NONE', 'WORKASPACE' ) );
#10533 = DIRECTION ( 'NONE',  ( 0.8820010751365676693, 0.000000000000000000, 0.4712473909295825658 ) ) ;
#10534 = CARTESIAN_POINT ( 'NONE',  ( 16.88587703871184331, -6.724495681871323072, -303.4999999999996589 ) ) ;
#10535 = EDGE_CURVE ( 'NONE', #8899, #9652, #3150, .T. ) ;
#10536 = CARTESIAN_POINT ( 'NONE',  ( 17.16710485141000220, 2.239552065056999997, -314.4150829855000211 ) ) ;
#10537 = CARTESIAN_POINT ( 'NONE',  ( 15.00000000000000000, 0.000000000000000000, -285.0000000000000000 ) ) ;
#10538 = CARTESIAN_POINT ( 'NONE',  ( -3.744595214114432746, -7.028316276732002876, -436.1346940467533955 ) ) ;
#10539 = CARTESIAN_POINT ( 'NONE',  ( -16.20020866270998638, 5.814836367836996978, 319.9928079742500131 ) ) ;
#10540 = CIRCLE ( 'NONE', #3675, 0.5000000000000004441 ) ;
#10541 = ORIENTED_EDGE ( 'NONE', *, *, #4779, .T. ) ;
#10542 = CARTESIAN_POINT ( 'NONE',  ( 12.80442074722001067, 9.608322671940996429, -316.3802825947000201 ) ) ;
#10543 = CARTESIAN_POINT ( 'NONE',  ( 6.751314262718001835, -11.77064546103999731, -316.3802825947000201 ) ) ;
#10544 = AXIS2_PLACEMENT_3D ( 'NONE', #4028, #4937, #3167 ) ;
#10545 = AXIS2_PLACEMENT_3D ( 'NONE', #1128, #4506, #6936 ) ;
#10546 = AXIS2_PLACEMENT_3D ( 'NONE', #3713, #4510, #8538 ) ;
#10547 = VERTEX_POINT ( 'NONE', #479 ) ;
#10548 = CARTESIAN_POINT ( 'NONE',  ( 12.48775874806000097, -8.649334263351001084, 320.0000000000000000 ) ) ;
#10549 = CARTESIAN_POINT ( 'NONE',  ( -0.7589204585291327021, -7.448615989627000999, -434.4456504183515335 ) ) ;
#10550 = PRODUCT_DEFINITION_CONTEXT ( 'detailed design', #9551, 'design' ) ;
#10551 = FACE_OUTER_BOUND ( 'NONE', #5690, .T. ) ;
#10552 = DIRECTION ( 'NONE',  ( 0.000000000000000000, 0.000000000000000000, -1.000000000000000000 ) ) ;
#10553 = CIRCLE ( 'NONE', #4378, 3.500000000000020428 ) ;
#10555 = ORIENTED_EDGE ( 'NONE', *, *, #3332, .T. ) ;
#10554 = PRESENTATION_LAYER_ASSIGNMENT (  '', '', ( #8325 ) ) ;
#10556 = CARTESIAN_POINT ( 'NONE',  ( -14.55942669488979391, -5.453671309400836442, -314.5801547934445352 ) ) ;
#10557 = ORIENTED_EDGE ( 'NONE', *, *, #181, .F. ) ;
#10558 = DIRECTION ( 'NONE',  ( -0.8820010751365675583, 0.000000000000000000, -0.4712473909295827323 ) ) ;
#10559 = ORIENTED_EDGE ( 'NONE', *, *, #493, .T. ) ;
#10560 = CARTESIAN_POINT ( 'NONE',  ( -2.545396798794703042, -9.391972178232515844, 315.0000000000000568 ) ) ;
#10561 = CARTESIAN_POINT ( 'NONE',  ( -3.644643686525998572, -11.88155656384000203, -302.4229045757450081 ) ) ;
#10562 = FACE_OUTER_BOUND ( 'NONE', #7570, .T. ) ;
#10563 = CARTESIAN_POINT ( 'NONE',  ( -72.90663470096859555, -7.500000000000000000, -371.7168990827444190 ) ) ;
#10564 = COLOUR_RGB ( '', 0.08235294, 0.09019608, 0.10196078) ;
#10565 = CARTESIAN_POINT ( 'NONE',  ( 12.62193639354000396, 9.236300292413996971, -302.4229045757450081 ) ) ;
#10566 = CARTESIAN_POINT ( 'NONE',  ( 9.526067998327799539E-10, -10.00000000005854339, 314.4999528359535361 ) ) ;
#10567 = VERTEX_POINT ( 'NONE', #7039 ) ;
#10568 = CARTESIAN_POINT ( 'NONE',  ( 12.07130791617000121, -6.858215270785999351, -314.8616023057000461 ) ) ;
#10569 = CARTESIAN_POINT ( 'NONE',  ( 19.99999036626000048, 4.642009117057000143E-09, -316.5000000000000000 ) ) ;
#10570 = ORIENTED_EDGE ( 'NONE', *, *, #3707, .F. ) ;
#10571 = CARTESIAN_POINT ( 'NONE',  ( -18.70165185342001735, -1.614428960665998503, 190.0071920248299477 ) ) ;
#10572 = CARTESIAN_POINT ( 'NONE',  ( 18.21004088691051948, 5.189404274100754222, 190.9999999999996589 ) ) ;
#10573 = CARTESIAN_POINT ( 'NONE',  ( -2.000000000000000000, -2.500000000000000000, -409.5000000000000568 ) ) ;
#10574 = PRESENTATION_LAYER_ASSIGNMENT (  '', '', ( #8171 ) ) ;
#10575 = CARTESIAN_POINT ( 'NONE',  ( 1.419551022038999966, -10.09154694854999867, 314.4150829855000211 ) ) ;
#10576 = CARTESIAN_POINT ( 'NONE',  ( 7.608551686289999338, 10.53686309807999955, 320.0000000000000000 ) ) ;
#10577 = CARTESIAN_POINT ( 'NONE',  ( -34.37192209820132405, -2.500000000000000000, -461.0868123482146643 ) ) ;
#10578 = CARTESIAN_POINT ( 'NONE',  ( 16.38421488526942582, 7.181844560322187654, 319.0000000000005116 ) ) ;
#10579 = CARTESIAN_POINT ( 'NONE',  ( -14.86799266576450584, -4.360433334866828936, -438.9019099114260030 ) ) ;
#10580 = CARTESIAN_POINT ( 'NONE',  ( -14.37110465573396212, -2.500000000000000000, -348.9812360766022721 ) ) ;
#10581 = ORIENTED_EDGE ( 'NONE', *, *, #5233, .F. ) ;
#10582 = DIRECTION ( 'NONE',  ( 0.000000000000000000, -1.000000000000000000, 0.000000000000000000 ) ) ;
#10583 = ORIENTED_EDGE ( 'NONE', *, *, #2143, .T. ) ;
#10584 = CARTESIAN_POINT ( 'NONE',  ( 19.99999036626000048, 4.642009117057000143E-09, -316.5000000000000000 ) ) ;
#10585 =( BOUNDED_CURVE ( )  B_SPLINE_CURVE ( 3, ( #7417, #3335, #3177, #3978 ),
 .UNSPECIFIED., .F., .F. ) 
 B_SPLINE_CURVE_WITH_KNOTS ( ( 4, 4 ),
 ( 0.000000000000000000, 1.000000000000000000 ),
 .UNSPECIFIED. ) 
 CURVE ( )  GEOMETRIC_REPRESENTATION_ITEM ( )  RATIONAL_B_SPLINE_CURVE ( ( 1.171566417337508881, 0.9428088753384672449, 0.9428111942444036275, 1.171573374055317807 ) ) 
 REPRESENTATION_ITEM ( '' )  );
#10586 = FACE_OUTER_BOUND ( 'NONE', #3212, .T. ) ;
#10587 = SHAPE_DEFINITION_REPRESENTATION ( #1506, #4085 ) ;
#10588 = CARTESIAN_POINT ( 'NONE',  ( 1.674130924758677086, -12.47364919270561856, -303.4999999999996589 ) ) ;
#10589 = CARTESIAN_POINT ( 'NONE',  ( 15.39920013370999996, 4.579805981517999669, -314.6383426456000052 ) ) ;
#10590 = FACE_OUTER_BOUND ( 'NONE', #8166, .T. ) ;
#10591 = FACE_OUTER_BOUND ( 'NONE', #2486, .T. ) ;
#10592 = CARTESIAN_POINT ( 'NONE',  ( 19.14248421182001891, 3.638193899013998145, 318.8802828394900644 ) ) ;
#10593 = CARTESIAN_POINT ( 'NONE',  ( -49.82771619714345235, -7.500000000000000000, -415.9731248673013511 ) ) ;
#10594 = CARTESIAN_POINT ( 'NONE',  ( -1.059650150527880585, -2.568636005655999366, -435.0577782176294477 ) ) ;
#10595 = LINE ( 'NONE', #3237, #7457 ) ;
#10596 = CARTESIAN_POINT ( 'NONE',  ( 17.77555462084998794, 5.884850558328997394, -317.0792622552969533 ) ) ;
#10597 = CARTESIAN_POINT ( 'NONE',  ( 5.321980890543003717, -12.05475797716000486, -316.3802825947000201 ) ) ;
#10598 = DIRECTION ( 'NONE',  ( -0.9712267471052612455, -0.000000000000000000, -0.2381566831044910626 ) ) ;
#10599 = CARTESIAN_POINT ( 'NONE',  ( -0.1726170993359143480, -7.634036073875003048, -434.4152387547379135 ) ) ;
#10600 = CIRCLE ( 'NONE', #1858, 0.5000000000000004441 ) ;
#10601 = DIRECTION ( 'NONE',  ( 2.716996281204025196E-06, -0.9999999999963090636, 3.949787424940705384E-23 ) ) ;
#10602 = CARTESIAN_POINT ( 'NONE',  ( 4.780493465650555329, -9.113006550021841790, -315.0000000000000568 ) ) ;
#10603 = ORIENTED_EDGE ( 'NONE', *, *, #3484, .F. ) ;
#10604 = CARTESIAN_POINT ( 'NONE',  ( 17.50000000000125056, 1.338989683019597976E-14, -315.0000000000000568 ) ) ;
#10605 = ORIENTED_EDGE ( 'NONE', *, *, #10029, .F. ) ;
#10606 = CARTESIAN_POINT ( 'NONE',  ( 8.891587890486999157, 10.15986303230000054, -317.5000000000000000 ) ) ;
#10607 = ORIENTED_EDGE ( 'NONE', *, *, #5217, .F. ) ;
#10608 = CARTESIAN_POINT ( 'NONE',  ( 20.05676974677001922, 0.5613724988767001545, -302.9207377450070453 ) ) ;
#10609 = ADVANCED_FACE ( 'NONE', ( #10410 ), #3806, .T. ) ;
#10610 = DIRECTION ( 'NONE',  ( 0.000000000000000000, 1.000000000000000000, -0.000000000000000000 ) ) ;
#10611 = ADVANCED_FACE ( 'NONE', ( #640, #10359, #8798, #1384 ), #2946, .T. ) ;
#10612 = CARTESIAN_POINT ( 'NONE',  ( -82.14476046060677561, -2.366295999999999733, -345.9384288226025888 ) ) ;
#10613 =( NAMED_UNIT ( * ) SI_UNIT ( $, .STERADIAN. ) SOLID_ANGLE_UNIT ( ) );
#10614 = CARTESIAN_POINT ( 'NONE',  ( -11.54867409098999964, 9.757628671089998207, -302.4229045757450081 ) ) ;
#10615 = LINE ( 'NONE', #1699, #1721 ) ;
#10616 = EDGE_LOOP ( 'NONE', ( #778, #416, #9962, #10238 ) ) ;
#10617 = DIRECTION ( 'NONE',  ( 0.000000000000000000, 1.000000000000000000, -0.000000000000000000 ) ) ;
#10618 = EDGE_CURVE ( 'NONE', #7113, #10046, #4727, .T. ) ;
#10619 = CARTESIAN_POINT ( 'NONE',  ( -3.672956643297854651, -2.683304555918673451, -435.3862750469904768 ) ) ;
#10620 = ORIENTED_EDGE ( 'NONE', *, *, #8488, .F. ) ;
#10621 = CARTESIAN_POINT ( 'NONE',  ( -17.32898823752001860, -5.623515075799002894, 189.9229057364800042 ) ) ;
#10622 = CARTESIAN_POINT ( 'NONE',  ( 15.60370682163541289, 7.832153051853420145, 190.9999999999996589 ) ) ;
#10623 = EDGE_CURVE ( 'NONE', #4592, #1010, #10177, .T. ) ;
#10624 = NEXT_ASSEMBLY_USAGE_OCCURRENCE ( 'NAUO1', ' ', ' ', #3963, #8885, $ ) ;
#10625 = NEXT_ASSEMBLY_USAGE_OCCURRENCE ( 'NAUO2', ' ', ' ', #3963, #286, $ ) ;
#10626 = NEXT_ASSEMBLY_USAGE_OCCURRENCE ( 'NAUO3', ' ', ' ', #3963, #6660, $ ) ;
#10627 = NEXT_ASSEMBLY_USAGE_OCCURRENCE ( 'NAUO4', ' ', ' ', #3963, #2191, $ ) ;
#10628 = NEXT_ASSEMBLY_USAGE_OCCURRENCE ( 'NAUO5', ' ', ' ', #3963, #8229, $ ) ;
#10629 = NEXT_ASSEMBLY_USAGE_OCCURRENCE ( 'NAUO6', ' ', ' ', #3963, #3305, $ ) ;
#10630 = NEXT_ASSEMBLY_USAGE_OCCURRENCE ( 'NAUO7', ' ', ' ', #3963, #2522, $ ) ;
#10631 = NEXT_ASSEMBLY_USAGE_OCCURRENCE ( 'NAUO8', ' ', ' ', #3963, #2387, $ ) ;
#10632 = NEXT_ASSEMBLY_USAGE_OCCURRENCE ( 'NAUO9', ' ', ' ', #3963, #8684, $ ) ;
#10633 = NEXT_ASSEMBLY_USAGE_OCCURRENCE ( 'NAUO10', ' ', ' ', #3963, #8885, $ ) ;
#10634 = NEXT_ASSEMBLY_USAGE_OCCURRENCE ( 'NAUO11', ' ', ' ', #3963, #8684, $ ) ;
#10635 = NEXT_ASSEMBLY_USAGE_OCCURRENCE ( 'NAUO12', ' ', ' ', #3963, #8885, $ ) ;
#10636 = NEXT_ASSEMBLY_USAGE_OCCURRENCE ( 'NAUO13', ' ', ' ', #3963, #8885, $ ) ;
#10637 = NEXT_ASSEMBLY_USAGE_OCCURRENCE ( 'NAUO14', ' ', ' ', #3963, #2387, $ ) ;
ENDSEC;
END-ISO-10303-21;
